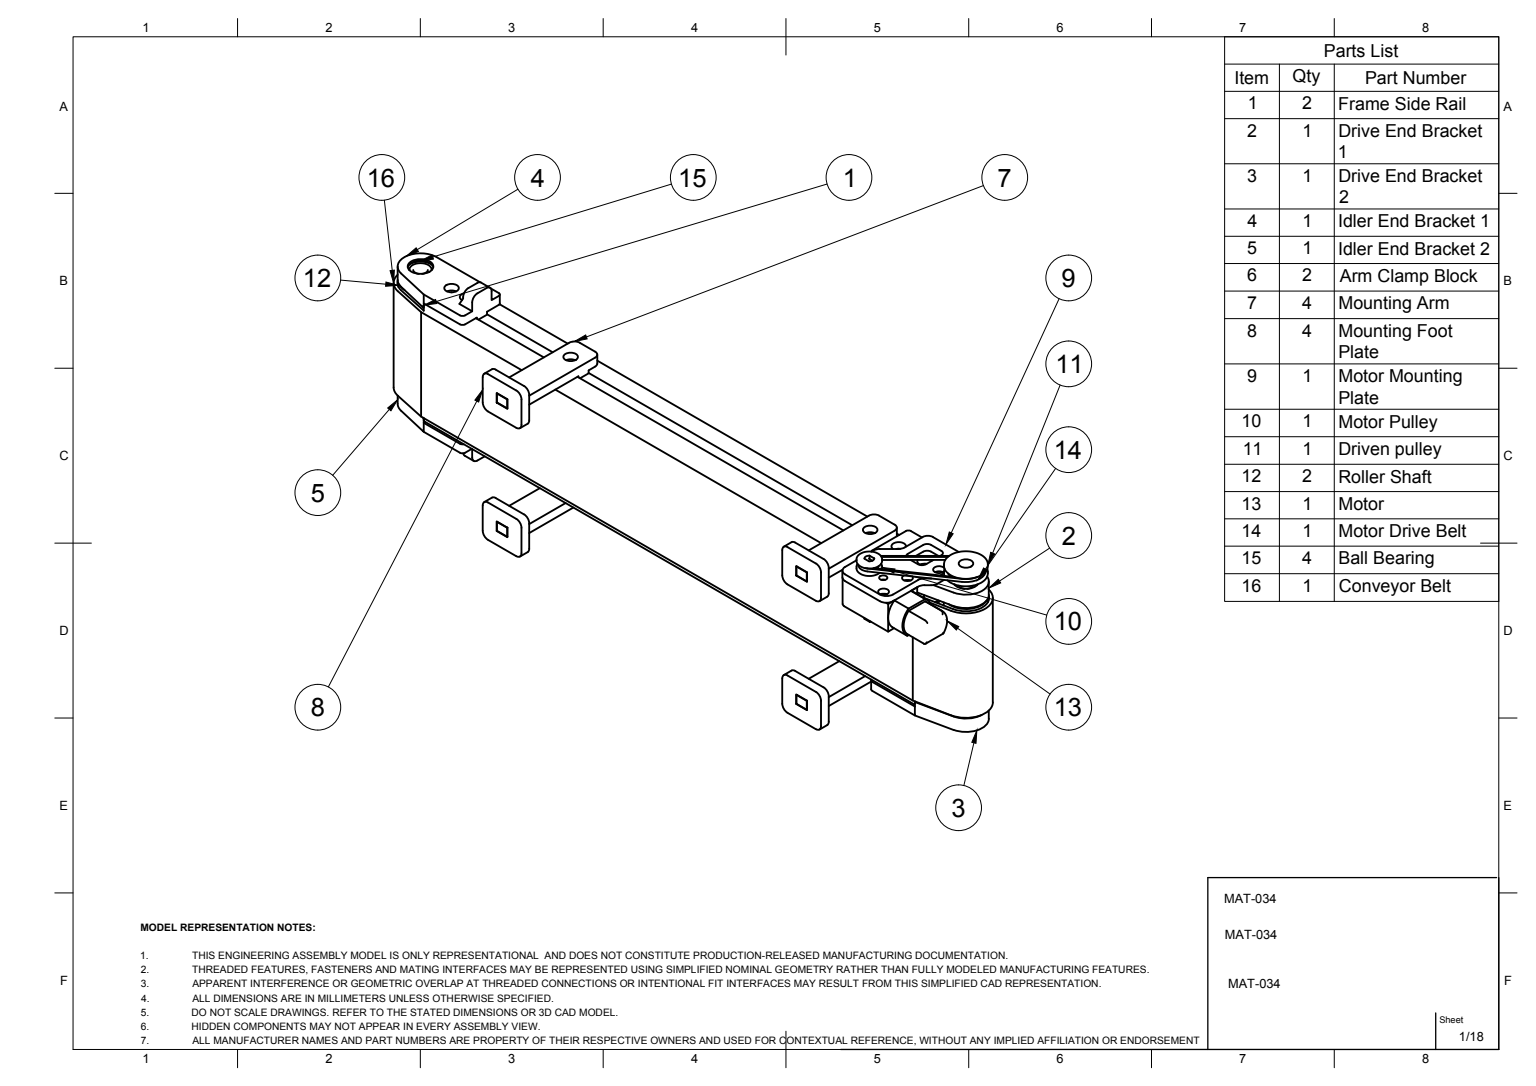
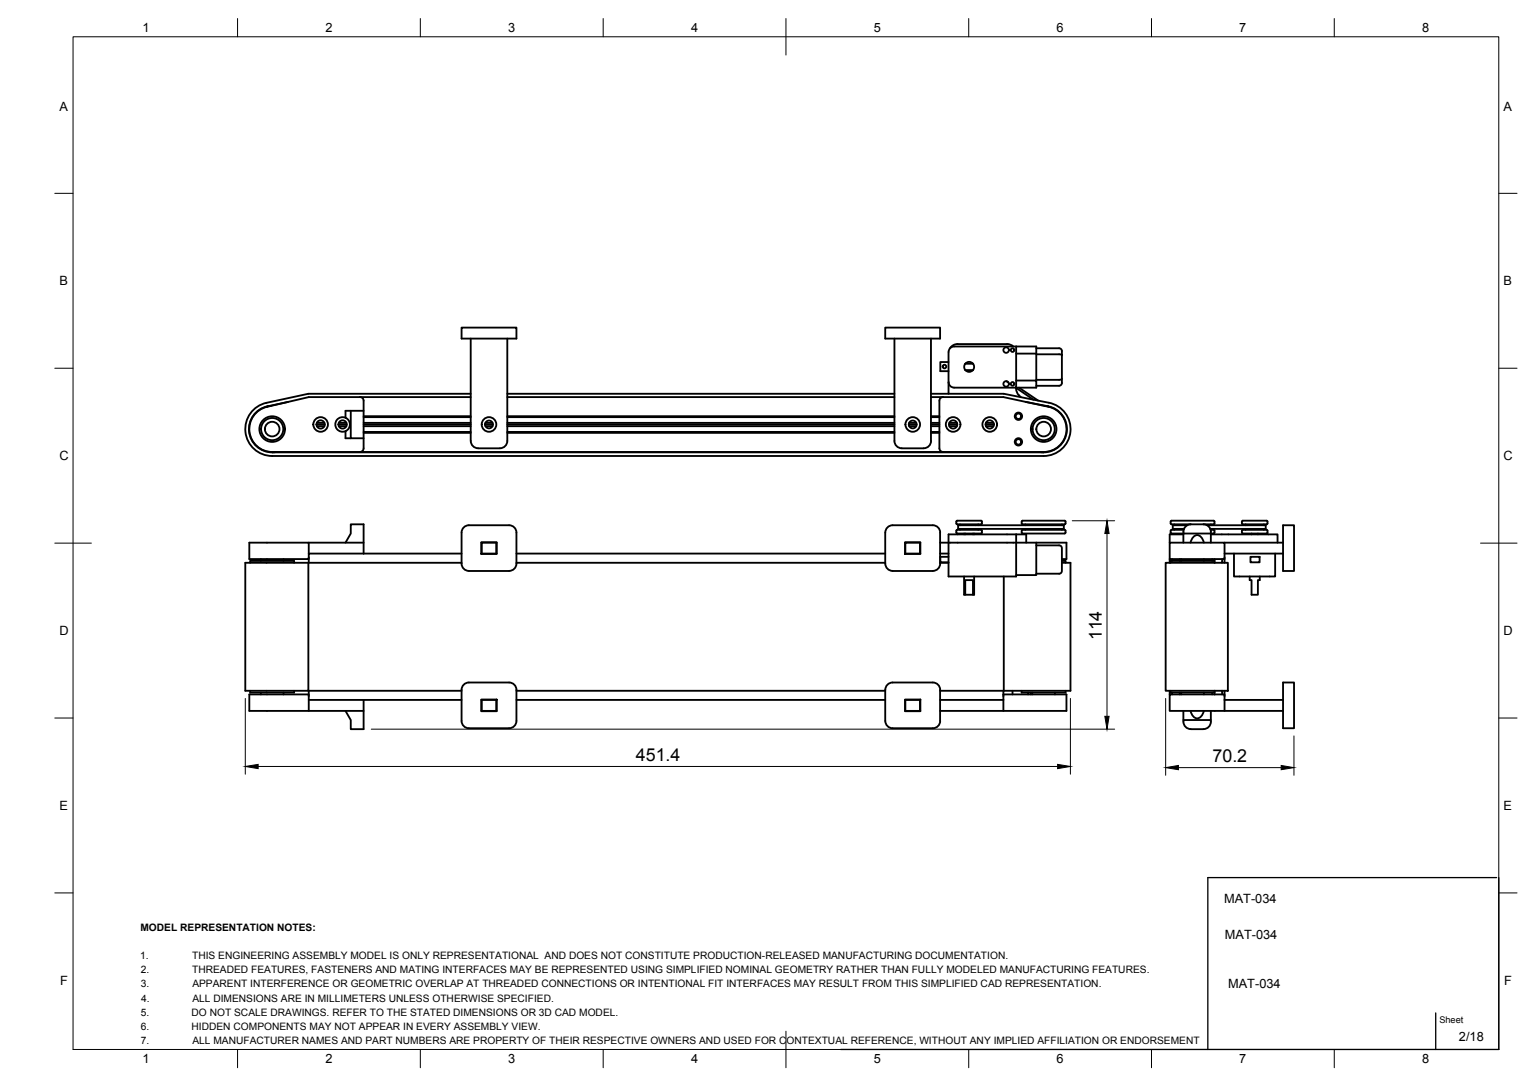
ISO-10303-21;
HEADER;
/* Generated by software containing ST-Developer
 * from STEP Tools, Inc. (www.steptools.com) 
 */

FILE_DESCRIPTION(
/* description */ ('STEP AP214'),
/* implementation_level */ '2;1');

FILE_NAME(
/* name */ 'MAT-034.step',
/* time_stamp */ '2026-11-14T09:24:36-08:00',
/* author */ (''),
/* organization */ (''),
/* preprocessor_version */ 'ST-DEVELOPER v20.2',
/* originating_system */ 'Autodesk Translation Framework v15.17.0.0',
/* authorisation */ '');

FILE_SCHEMA (('AUTOMOTIVE_DESIGN { 1 0 10303 214 3 1 1 }'));
ENDSEC;

DATA;
#10=MECHANICAL_DESIGN_GEOMETRIC_PRESENTATION_REPRESENTATION('',(#203,#204,
#205,#206,#207,#208,#209,#210,#211,#212,#213,#214,#215,#216,#217,#218,#219,
#220,#221,#222,#223,#224,#225,#226),#18867);
#11=ITEM_DEFINED_TRANSFORMATION($,$,#11712,#12275);
#12=ITEM_DEFINED_TRANSFORMATION($,$,#11160,#12276);
#13=ITEM_DEFINED_TRANSFORMATION($,$,#11233,#12277);
#14=ITEM_DEFINED_TRANSFORMATION($,$,#11306,#12278);
#15=ITEM_DEFINED_TRANSFORMATION($,$,#11366,#12279);
#16=ITEM_DEFINED_TRANSFORMATION($,$,#12015,#12280);
#17=ITEM_DEFINED_TRANSFORMATION($,$,#12084,#12281);
#18=ITEM_DEFINED_TRANSFORMATION($,$,#12112,#12282);
#19=ITEM_DEFINED_TRANSFORMATION($,$,#11426,#12283);
#20=ITEM_DEFINED_TRANSFORMATION($,$,#11511,#12284);
#21=ITEM_DEFINED_TRANSFORMATION($,$,#11547,#12285);
#22=ITEM_DEFINED_TRANSFORMATION($,$,#12135,#12286);
#23=ITEM_DEFINED_TRANSFORMATION($,$,#11578,#12287);
#24=ITEM_DEFINED_TRANSFORMATION($,$,#11670,#12288);
#25=ITEM_DEFINED_TRANSFORMATION($,$,#12163,#12289);
#26=ITEM_DEFINED_TRANSFORMATION($,$,#11689,#12290);
#27=ITEM_DEFINED_TRANSFORMATION($,$,#11712,#12291);
#28=ITEM_DEFINED_TRANSFORMATION($,$,#12015,#12292);
#29=ITEM_DEFINED_TRANSFORMATION($,$,#12084,#12293);
#30=ITEM_DEFINED_TRANSFORMATION($,$,#12084,#12294);
#31=ITEM_DEFINED_TRANSFORMATION($,$,#12084,#12295);
#32=ITEM_DEFINED_TRANSFORMATION($,$,#12112,#12296);
#33=ITEM_DEFINED_TRANSFORMATION($,$,#12112,#12297);
#34=ITEM_DEFINED_TRANSFORMATION($,$,#12112,#12298);
#35=ITEM_DEFINED_TRANSFORMATION($,$,#12135,#12299);
#36=ITEM_DEFINED_TRANSFORMATION($,$,#12163,#12300);
#37=ITEM_DEFINED_TRANSFORMATION($,$,#12163,#12301);
#38=ITEM_DEFINED_TRANSFORMATION($,$,#12163,#12302);
#39=(
REPRESENTATION_RELATIONSHIP($,$,#18945,#18934)
REPRESENTATION_RELATIONSHIP_WITH_TRANSFORMATION(#11)
SHAPE_REPRESENTATION_RELATIONSHIP()
);
#40=(
REPRESENTATION_RELATIONSHIP($,$,#18935,#18934)
REPRESENTATION_RELATIONSHIP_WITH_TRANSFORMATION(#12)
SHAPE_REPRESENTATION_RELATIONSHIP()
);
#41=(
REPRESENTATION_RELATIONSHIP($,$,#18936,#18934)
REPRESENTATION_RELATIONSHIP_WITH_TRANSFORMATION(#13)
SHAPE_REPRESENTATION_RELATIONSHIP()
);
#42=(
REPRESENTATION_RELATIONSHIP($,$,#18937,#18934)
REPRESENTATION_RELATIONSHIP_WITH_TRANSFORMATION(#14)
SHAPE_REPRESENTATION_RELATIONSHIP()
);
#43=(
REPRESENTATION_RELATIONSHIP($,$,#18938,#18934)
REPRESENTATION_RELATIONSHIP_WITH_TRANSFORMATION(#15)
SHAPE_REPRESENTATION_RELATIONSHIP()
);
#44=(
REPRESENTATION_RELATIONSHIP($,$,#18946,#18934)
REPRESENTATION_RELATIONSHIP_WITH_TRANSFORMATION(#16)
SHAPE_REPRESENTATION_RELATIONSHIP()
);
#45=(
REPRESENTATION_RELATIONSHIP($,$,#18947,#18934)
REPRESENTATION_RELATIONSHIP_WITH_TRANSFORMATION(#17)
SHAPE_REPRESENTATION_RELATIONSHIP()
);
#46=(
REPRESENTATION_RELATIONSHIP($,$,#18948,#18934)
REPRESENTATION_RELATIONSHIP_WITH_TRANSFORMATION(#18)
SHAPE_REPRESENTATION_RELATIONSHIP()
);
#47=(
REPRESENTATION_RELATIONSHIP($,$,#18939,#18934)
REPRESENTATION_RELATIONSHIP_WITH_TRANSFORMATION(#19)
SHAPE_REPRESENTATION_RELATIONSHIP()
);
#48=(
REPRESENTATION_RELATIONSHIP($,$,#18940,#18934)
REPRESENTATION_RELATIONSHIP_WITH_TRANSFORMATION(#20)
SHAPE_REPRESENTATION_RELATIONSHIP()
);
#49=(
REPRESENTATION_RELATIONSHIP($,$,#18941,#18934)
REPRESENTATION_RELATIONSHIP_WITH_TRANSFORMATION(#21)
SHAPE_REPRESENTATION_RELATIONSHIP()
);
#50=(
REPRESENTATION_RELATIONSHIP($,$,#18949,#18934)
REPRESENTATION_RELATIONSHIP_WITH_TRANSFORMATION(#22)
SHAPE_REPRESENTATION_RELATIONSHIP()
);
#51=(
REPRESENTATION_RELATIONSHIP($,$,#18942,#18934)
REPRESENTATION_RELATIONSHIP_WITH_TRANSFORMATION(#23)
SHAPE_REPRESENTATION_RELATIONSHIP()
);
#52=(
REPRESENTATION_RELATIONSHIP($,$,#18943,#18934)
REPRESENTATION_RELATIONSHIP_WITH_TRANSFORMATION(#24)
SHAPE_REPRESENTATION_RELATIONSHIP()
);
#53=(
REPRESENTATION_RELATIONSHIP($,$,#18950,#18934)
REPRESENTATION_RELATIONSHIP_WITH_TRANSFORMATION(#25)
SHAPE_REPRESENTATION_RELATIONSHIP()
);
#54=(
REPRESENTATION_RELATIONSHIP($,$,#18944,#18934)
REPRESENTATION_RELATIONSHIP_WITH_TRANSFORMATION(#26)
SHAPE_REPRESENTATION_RELATIONSHIP()
);
#55=(
REPRESENTATION_RELATIONSHIP($,$,#18945,#18934)
REPRESENTATION_RELATIONSHIP_WITH_TRANSFORMATION(#27)
SHAPE_REPRESENTATION_RELATIONSHIP()
);
#56=(
REPRESENTATION_RELATIONSHIP($,$,#18946,#18934)
REPRESENTATION_RELATIONSHIP_WITH_TRANSFORMATION(#28)
SHAPE_REPRESENTATION_RELATIONSHIP()
);
#57=(
REPRESENTATION_RELATIONSHIP($,$,#18947,#18934)
REPRESENTATION_RELATIONSHIP_WITH_TRANSFORMATION(#29)
SHAPE_REPRESENTATION_RELATIONSHIP()
);
#58=(
REPRESENTATION_RELATIONSHIP($,$,#18947,#18934)
REPRESENTATION_RELATIONSHIP_WITH_TRANSFORMATION(#30)
SHAPE_REPRESENTATION_RELATIONSHIP()
);
#59=(
REPRESENTATION_RELATIONSHIP($,$,#18947,#18934)
REPRESENTATION_RELATIONSHIP_WITH_TRANSFORMATION(#31)
SHAPE_REPRESENTATION_RELATIONSHIP()
);
#60=(
REPRESENTATION_RELATIONSHIP($,$,#18948,#18934)
REPRESENTATION_RELATIONSHIP_WITH_TRANSFORMATION(#32)
SHAPE_REPRESENTATION_RELATIONSHIP()
);
#61=(
REPRESENTATION_RELATIONSHIP($,$,#18948,#18934)
REPRESENTATION_RELATIONSHIP_WITH_TRANSFORMATION(#33)
SHAPE_REPRESENTATION_RELATIONSHIP()
);
#62=(
REPRESENTATION_RELATIONSHIP($,$,#18948,#18934)
REPRESENTATION_RELATIONSHIP_WITH_TRANSFORMATION(#34)
SHAPE_REPRESENTATION_RELATIONSHIP()
);
#63=(
REPRESENTATION_RELATIONSHIP($,$,#18949,#18934)
REPRESENTATION_RELATIONSHIP_WITH_TRANSFORMATION(#35)
SHAPE_REPRESENTATION_RELATIONSHIP()
);
#64=(
REPRESENTATION_RELATIONSHIP($,$,#18950,#18934)
REPRESENTATION_RELATIONSHIP_WITH_TRANSFORMATION(#36)
SHAPE_REPRESENTATION_RELATIONSHIP()
);
#65=(
REPRESENTATION_RELATIONSHIP($,$,#18950,#18934)
REPRESENTATION_RELATIONSHIP_WITH_TRANSFORMATION(#37)
SHAPE_REPRESENTATION_RELATIONSHIP()
);
#66=(
REPRESENTATION_RELATIONSHIP($,$,#18950,#18934)
REPRESENTATION_RELATIONSHIP_WITH_TRANSFORMATION(#38)
SHAPE_REPRESENTATION_RELATIONSHIP()
);
#67=CONTEXT_DEPENDENT_SHAPE_REPRESENTATION(#39,#18906);
#68=CONTEXT_DEPENDENT_SHAPE_REPRESENTATION(#40,#18907);
#69=CONTEXT_DEPENDENT_SHAPE_REPRESENTATION(#41,#18908);
#70=CONTEXT_DEPENDENT_SHAPE_REPRESENTATION(#42,#18909);
#71=CONTEXT_DEPENDENT_SHAPE_REPRESENTATION(#43,#18910);
#72=CONTEXT_DEPENDENT_SHAPE_REPRESENTATION(#44,#18911);
#73=CONTEXT_DEPENDENT_SHAPE_REPRESENTATION(#45,#18912);
#74=CONTEXT_DEPENDENT_SHAPE_REPRESENTATION(#46,#18913);
#75=CONTEXT_DEPENDENT_SHAPE_REPRESENTATION(#47,#18914);
#76=CONTEXT_DEPENDENT_SHAPE_REPRESENTATION(#48,#18915);
#77=CONTEXT_DEPENDENT_SHAPE_REPRESENTATION(#49,#18916);
#78=CONTEXT_DEPENDENT_SHAPE_REPRESENTATION(#50,#18917);
#79=CONTEXT_DEPENDENT_SHAPE_REPRESENTATION(#51,#18918);
#80=CONTEXT_DEPENDENT_SHAPE_REPRESENTATION(#52,#18919);
#81=CONTEXT_DEPENDENT_SHAPE_REPRESENTATION(#53,#18920);
#82=CONTEXT_DEPENDENT_SHAPE_REPRESENTATION(#54,#18921);
#83=CONTEXT_DEPENDENT_SHAPE_REPRESENTATION(#55,#18922);
#84=CONTEXT_DEPENDENT_SHAPE_REPRESENTATION(#56,#18923);
#85=CONTEXT_DEPENDENT_SHAPE_REPRESENTATION(#57,#18924);
#86=CONTEXT_DEPENDENT_SHAPE_REPRESENTATION(#58,#18925);
#87=CONTEXT_DEPENDENT_SHAPE_REPRESENTATION(#59,#18926);
#88=CONTEXT_DEPENDENT_SHAPE_REPRESENTATION(#60,#18927);
#89=CONTEXT_DEPENDENT_SHAPE_REPRESENTATION(#61,#18928);
#90=CONTEXT_DEPENDENT_SHAPE_REPRESENTATION(#62,#18929);
#91=CONTEXT_DEPENDENT_SHAPE_REPRESENTATION(#63,#18930);
#92=CONTEXT_DEPENDENT_SHAPE_REPRESENTATION(#64,#18931);
#93=CONTEXT_DEPENDENT_SHAPE_REPRESENTATION(#65,#18932);
#94=CONTEXT_DEPENDENT_SHAPE_REPRESENTATION(#66,#18933);
#95=NEXT_ASSEMBLY_USAGE_OCCURRENCE('Frame Side Rail:1',
'Frame Side Rail:1','Frame Side Rail:1',#18952,#18963,
'Frame Side Rail:1');
#96=NEXT_ASSEMBLY_USAGE_OCCURRENCE('Drive End Bracket 1:1',
'Drive End Bracket 1:1','Drive End Bracket 1:1',#18952,#18953,
'Drive End Bracket 1:1');
#97=NEXT_ASSEMBLY_USAGE_OCCURRENCE('Drive End Bracket 2:1',
'Drive End Bracket 2:1','Drive End Bracket 2:1',#18952,#18954,
'Drive End Bracket 2:1');
#98=NEXT_ASSEMBLY_USAGE_OCCURRENCE('Idler End Bracket 1:1',
'Idler End Bracket 1:1','Idler End Bracket 1:1',#18952,#18955,
'Idler End Bracket 1:1');
#99=NEXT_ASSEMBLY_USAGE_OCCURRENCE('Idler End Bracket 2:1',
'Idler End Bracket 2:1','Idler End Bracket 2:1',#18952,#18956,
'Idler End Bracket 2:1');
#100=NEXT_ASSEMBLY_USAGE_OCCURRENCE('Arm Clamp Block:1',
'Arm Clamp Block:1','Arm Clamp Block:1',#18952,#18964,
'Arm Clamp Block:1');
#101=NEXT_ASSEMBLY_USAGE_OCCURRENCE('Mounting Arm:1','Mounting Arm:1',
'Mounting Arm:1',#18952,#18965,'Mounting Arm:1');
#102=NEXT_ASSEMBLY_USAGE_OCCURRENCE('Mounting Foot Plate:1',
'Mounting Foot Plate:1','Mounting Foot Plate:1',#18952,#18966,
'Mounting Foot Plate:1');
#103=NEXT_ASSEMBLY_USAGE_OCCURRENCE('Motor Mounting Plate:1',
'Motor Mounting Plate:1','Motor Mounting Plate:1',#18952,#18957,
'Motor Mounting Plate:1');
#104=NEXT_ASSEMBLY_USAGE_OCCURRENCE('Motor Pulley:1','Motor Pulley:1',
'Motor Pulley:1',#18952,#18958,'Motor Pulley:1');
#105=NEXT_ASSEMBLY_USAGE_OCCURRENCE('Driven Pulley:1','Driven Pulley:1',
'Driven Pulley:1',#18952,#18959,'Driven Pulley:1');
#106=NEXT_ASSEMBLY_USAGE_OCCURRENCE('Roller Shaft:1','Roller Shaft:1',
'Roller Shaft:1',#18952,#18967,'Roller Shaft:1');
#107=NEXT_ASSEMBLY_USAGE_OCCURRENCE('Motor:1','Motor:1','Motor:1',#18952,
#18960,'Motor:1');
#108=NEXT_ASSEMBLY_USAGE_OCCURRENCE('Motor Drive Belt:1',
'Motor Drive Belt:1','Motor Drive Belt:1',#18952,#18961,
'Motor Drive Belt:1');
#109=NEXT_ASSEMBLY_USAGE_OCCURRENCE('Ball Bearing:1','Ball Bearing:1',
'Ball Bearing:1',#18952,#18968,'Ball Bearing:1');
#110=NEXT_ASSEMBLY_USAGE_OCCURRENCE('Conveyor Belt:1','Conveyor Belt:1',
'Conveyor Belt:1',#18952,#18962,'Conveyor Belt:1');
#111=NEXT_ASSEMBLY_USAGE_OCCURRENCE('Frame Side Rail:2',
'Frame Side Rail:2','Frame Side Rail:2',#18952,#18963,
'Frame Side Rail:2');
#112=NEXT_ASSEMBLY_USAGE_OCCURRENCE('Arm Clamp Block:2',
'Arm Clamp Block:2','Arm Clamp Block:2',#18952,#18964,
'Arm Clamp Block:2');
#113=NEXT_ASSEMBLY_USAGE_OCCURRENCE('Mounting Arm:2','Mounting Arm:2',
'Mounting Arm:2',#18952,#18965,'Mounting Arm:2');
#114=NEXT_ASSEMBLY_USAGE_OCCURRENCE('Mounting Arm:3','Mounting Arm:3',
'Mounting Arm:3',#18952,#18965,'Mounting Arm:3');
#115=NEXT_ASSEMBLY_USAGE_OCCURRENCE('Mounting Arm:4','Mounting Arm:4',
'Mounting Arm:4',#18952,#18965,'Mounting Arm:4');
#116=NEXT_ASSEMBLY_USAGE_OCCURRENCE('Mounting Foot Plate:2',
'Mounting Foot Plate:2','Mounting Foot Plate:2',#18952,#18966,
'Mounting Foot Plate:2');
#117=NEXT_ASSEMBLY_USAGE_OCCURRENCE('Mounting Foot Plate:3',
'Mounting Foot Plate:3','Mounting Foot Plate:3',#18952,#18966,
'Mounting Foot Plate:3');
#118=NEXT_ASSEMBLY_USAGE_OCCURRENCE('Mounting Foot Plate:4',
'Mounting Foot Plate:4','Mounting Foot Plate:4',#18952,#18966,
'Mounting Foot Plate:4');
#119=NEXT_ASSEMBLY_USAGE_OCCURRENCE('Roller Shaft:2','Roller Shaft:2',
'Roller Shaft:2',#18952,#18967,'Roller Shaft:2');
#120=NEXT_ASSEMBLY_USAGE_OCCURRENCE('Ball Bearing:2','Ball Bearing:2',
'Ball Bearing:2',#18952,#18968,'Ball Bearing:2');
#121=NEXT_ASSEMBLY_USAGE_OCCURRENCE('Ball Bearing:3','Ball Bearing:3',
'Ball Bearing:3',#18952,#18968,'Ball Bearing:3');
#122=NEXT_ASSEMBLY_USAGE_OCCURRENCE('Ball Bearing:4','Ball Bearing:4',
'Ball Bearing:4',#18952,#18968,'Ball Bearing:4');
#123=SPHERICAL_SURFACE('',#12164,1.9845);
#124=SPHERICAL_SURFACE('',#12166,1.9845);
#125=SPHERICAL_SURFACE('',#12168,1.9845);
#126=SPHERICAL_SURFACE('',#12170,1.9845);
#127=SPHERICAL_SURFACE('',#12172,1.9845);
#128=SPHERICAL_SURFACE('',#12174,1.9845);
#129=SPHERICAL_SURFACE('',#12176,1.9845);
#130=CONICAL_SURFACE('',#12139,12.7,0.0194419944400805);
#131=CONICAL_SURFACE('',#12143,12.7,0.0194419944400803);
#132=CONICAL_SURFACE('',#12193,8.8,1.39626340159546);
#133=CONICAL_SURFACE('',#12203,9.6,1.39626340159547);
#134=CONICAL_SURFACE('',#12217,9.6,1.46902152746005);
#135=CONICAL_SURFACE('',#12222,8.71875,1.51977681092793);
#136=CONICAL_SURFACE('',#12225,7.8375,1.51977681092793);
#137=CONICAL_SURFACE('',#12227,7.8375,1.51977681092793);
#138=CONICAL_SURFACE('',#12231,8.71875,1.46902152746005);
#139=CONICAL_SURFACE('',#12235,6.075,1.51977681092793);
#140=CONICAL_SURFACE('',#12238,8.71875,1.51977681092792);
#141=CONICAL_SURFACE('',#12242,9.6,1.51977681092792);
#142=B_SPLINE_CURVE_WITH_KNOTS('',3,(#16841,#16842,#16843,#16844,#16845,
#16846,#16847,#16848,#16849,#16850,#16851,#16852,#16853,#16854),
 .UNSPECIFIED.,.F.,.F.,(4,2,2,2,2,2,4),(0.245799129465821,0.300704982929502,
0.357513955396153,0.418543136612542,0.45489286030411,0.491598258931638,
0.492200531214483),.UNSPECIFIED.);
#143=B_SPLINE_CURVE_WITH_KNOTS('',3,(#16857,#16858,#16859,#16860,#16861,
#16862,#16863,#16864,#16865,#16866,#16867,#16868,#16869,#16870),
 .UNSPECIFIED.,.F.,.F.,(4,2,2,2,2,2,4),(-0.243764588636152,-0.188160877929009,
-0.130985417478992,-0.0703706382818566,-0.0353193180725583,0.,0.000595335954832901),
 .UNSPECIFIED.);
#144=B_SPLINE_CURVE_WITH_KNOTS('',3,(#17002,#17003,#17004,#17005,#17006,
#17007,#17008,#17009,#17010,#17011,#17012,#17013,#17014,#17015),
 .UNSPECIFIED.,.F.,.F.,(4,2,2,2,2,2,4),(-0.000602272282836634,0.,0.0367053986270638,
0.0730551223181225,0.134084303533662,0.190893275999521,0.245799129462431),
 .UNSPECIFIED.);
#145=B_SPLINE_CURVE_WITH_KNOTS('',3,(#17017,#17018,#17019,#17020,#17021,
#17022,#17023,#17024,#17025,#17026,#17027,#17028,#17029,#17030),
 .UNSPECIFIED.,.F.,.F.,(4,2,2,2,2,2,4),(-0.488124513225642,-0.487529177270534,
-0.452209859198347,-0.417158538989302,-0.356543759792373,-0.299368299342555,
-0.243764588635598),.UNSPECIFIED.);
#146=TOROIDAL_SURFACE('',#11512,6.5,0.5);
#147=TOROIDAL_SURFACE('',#11516,6.5,0.5);
#148=TOROIDAL_SURFACE('',#11521,6.5,0.5);
#149=TOROIDAL_SURFACE('',#11525,6.5,0.5);
#150=TOROIDAL_SURFACE('',#11551,11.5,0.5);
#151=TOROIDAL_SURFACE('',#11555,11.5,0.5);
#152=TOROIDAL_SURFACE('',#11560,11.5,0.5);
#153=TOROIDAL_SURFACE('',#11564,11.5,0.5);
#154=TOROIDAL_SURFACE('',#11579,1.8,0.2);
#155=TOROIDAL_SURFACE('',#11608,8.75000000000038,1.5);
#156=TOROIDAL_SURFACE('',#11653,8.75000000000038,1.5);
#157=TOROIDAL_SURFACE('',#12178,10.7,0.3);
#158=TOROIDAL_SURFACE('',#12184,10.7,0.3);
#159=TOROIDAL_SURFACE('',#12190,9.6,0.18);
#160=TOROIDAL_SURFACE('',#12197,7.35,1.9845);
#161=TOROIDAL_SURFACE('',#12206,9.6,0.18);
#162=TOROIDAL_SURFACE('',#12213,7.35,1.9845);
#163=TOROIDAL_SURFACE('',#12250,5.975,0.1);
#164=TOROIDAL_SURFACE('',#12253,4.3,0.3);
#165=TOROIDAL_SURFACE('',#12259,4.3,0.3);
#166=TOROIDAL_SURFACE('',#12262,5.975,0.1);
#167=ELLIPSE('',#11309,7.99999999999913,3.99999999999963);
#168=ELLIPSE('',#11311,7.99999999999913,3.99999999999963);
#169=ELLIPSE('',#11369,7.99999999999924,3.99999999999989);
#170=ELLIPSE('',#11371,7.99999999999924,3.99999999999989);
#171=SHAPE_REPRESENTATION_RELATIONSHIP('SRR','None',#18935,#187);
#172=SHAPE_REPRESENTATION_RELATIONSHIP('SRR','None',#18936,#188);
#173=SHAPE_REPRESENTATION_RELATIONSHIP('SRR','None',#18937,#189);
#174=SHAPE_REPRESENTATION_RELATIONSHIP('SRR','None',#18938,#190);
#175=SHAPE_REPRESENTATION_RELATIONSHIP('SRR','None',#18939,#191);
#176=SHAPE_REPRESENTATION_RELATIONSHIP('SRR','None',#18940,#192);
#177=SHAPE_REPRESENTATION_RELATIONSHIP('SRR','None',#18941,#193);
#178=SHAPE_REPRESENTATION_RELATIONSHIP('SRR','None',#18942,#194);
#179=SHAPE_REPRESENTATION_RELATIONSHIP('SRR','None',#18943,#195);
#180=SHAPE_REPRESENTATION_RELATIONSHIP('SRR','None',#18944,#196);
#181=SHAPE_REPRESENTATION_RELATIONSHIP('SRR','None',#18945,#197);
#182=SHAPE_REPRESENTATION_RELATIONSHIP('SRR','None',#18946,#198);
#183=SHAPE_REPRESENTATION_RELATIONSHIP('SRR','None',#18947,#199);
#184=SHAPE_REPRESENTATION_RELATIONSHIP('SRR','None',#18948,#200);
#185=SHAPE_REPRESENTATION_RELATIONSHIP('SRR','None',#18949,#201);
#186=SHAPE_REPRESENTATION_RELATIONSHIP('SRR','None',#18950,#202);
#187=ADVANCED_BREP_SHAPE_REPRESENTATION('',(#227),#18851);
#188=ADVANCED_BREP_SHAPE_REPRESENTATION('',(#228),#18852);
#189=ADVANCED_BREP_SHAPE_REPRESENTATION('',(#229),#18853);
#190=ADVANCED_BREP_SHAPE_REPRESENTATION('',(#230),#18854);
#191=ADVANCED_BREP_SHAPE_REPRESENTATION('',(#231),#18855);
#192=ADVANCED_BREP_SHAPE_REPRESENTATION('',(#232),#18856);
#193=ADVANCED_BREP_SHAPE_REPRESENTATION('',(#233),#18857);
#194=ADVANCED_BREP_SHAPE_REPRESENTATION('',(#234),#18858);
#195=ADVANCED_BREP_SHAPE_REPRESENTATION('',(#235),#18859);
#196=ADVANCED_BREP_SHAPE_REPRESENTATION('',(#236),#18860);
#197=ADVANCED_BREP_SHAPE_REPRESENTATION('',(#237),#18861);
#198=ADVANCED_BREP_SHAPE_REPRESENTATION('',(#238),#18862);
#199=ADVANCED_BREP_SHAPE_REPRESENTATION('',(#239),#18863);
#200=ADVANCED_BREP_SHAPE_REPRESENTATION('',(#240),#18864);
#201=ADVANCED_BREP_SHAPE_REPRESENTATION('',(#241),#18865);
#202=ADVANCED_BREP_SHAPE_REPRESENTATION('',(#242,#243,#244,#245,#246,#247,
#248,#249,#250),#18866);
#203=STYLED_ITEM('',(#19024),#227);
#204=STYLED_ITEM('',(#19024),#228);
#205=STYLED_ITEM('',(#19024),#229);
#206=STYLED_ITEM('',(#19025),#230);
#207=STYLED_ITEM('',(#19026),#231);
#208=STYLED_ITEM('',(#19027),#232);
#209=STYLED_ITEM('',(#19027),#233);
#210=STYLED_ITEM('',(#19026),#234);
#211=STYLED_ITEM('',(#19028),#235);
#212=STYLED_ITEM('',(#19028),#236);
#213=STYLED_ITEM('',(#19024),#237);
#214=STYLED_ITEM('',(#19026),#238);
#215=STYLED_ITEM('',(#19026),#239);
#216=STYLED_ITEM('',(#19024),#240);
#217=STYLED_ITEM('',(#19027),#241);
#218=STYLED_ITEM('',(#19027),#242);
#219=STYLED_ITEM('',(#19027),#243);
#220=STYLED_ITEM('',(#19027),#244);
#221=STYLED_ITEM('',(#19027),#245);
#222=STYLED_ITEM('',(#19027),#246);
#223=STYLED_ITEM('',(#19027),#247);
#224=STYLED_ITEM('',(#19027),#248);
#225=STYLED_ITEM('',(#19027),#249);
#226=STYLED_ITEM('',(#19027),#250);
#227=MANIFOLD_SOLID_BREP('Body1',#10958);
#228=MANIFOLD_SOLID_BREP('Body1',#10959);
#229=MANIFOLD_SOLID_BREP('Body1',#10960);
#230=MANIFOLD_SOLID_BREP('Body1',#10961);
#231=MANIFOLD_SOLID_BREP('Body1',#10962);
#232=MANIFOLD_SOLID_BREP('Body1',#10963);
#233=MANIFOLD_SOLID_BREP('Body1',#10964);
#234=MANIFOLD_SOLID_BREP('Body1',#10965);
#235=MANIFOLD_SOLID_BREP('Body1',#10966);
#236=MANIFOLD_SOLID_BREP('Body1',#10967);
#237=MANIFOLD_SOLID_BREP('Body1',#10968);
#238=MANIFOLD_SOLID_BREP('Body1',#10969);
#239=MANIFOLD_SOLID_BREP('Body1',#10970);
#240=MANIFOLD_SOLID_BREP('Body1',#10971);
#241=MANIFOLD_SOLID_BREP('Body1',#10972);
#242=MANIFOLD_SOLID_BREP('Body1',#10973);
#243=MANIFOLD_SOLID_BREP('Body2',#10974);
#244=MANIFOLD_SOLID_BREP('Body3',#10975);
#245=MANIFOLD_SOLID_BREP('Body4',#10976);
#246=MANIFOLD_SOLID_BREP('Body5',#10977);
#247=MANIFOLD_SOLID_BREP('Body6',#10978);
#248=MANIFOLD_SOLID_BREP('Body7',#10979);
#249=MANIFOLD_SOLID_BREP('Body8',#10980);
#250=MANIFOLD_SOLID_BREP('Body9',#10981);
#251=FACE_BOUND('',#1334,.T.);
#252=FACE_BOUND('',#1335,.T.);
#253=FACE_BOUND('',#1336,.T.);
#254=FACE_BOUND('',#1343,.T.);
#255=FACE_BOUND('',#1344,.T.);
#256=FACE_BOUND('',#1345,.T.);
#257=FACE_BOUND('',#1346,.T.);
#258=FACE_BOUND('',#1347,.T.);
#259=FACE_BOUND('',#1349,.T.);
#260=FACE_BOUND('',#1351,.T.);
#261=FACE_BOUND('',#1358,.T.);
#262=FACE_BOUND('',#1360,.T.);
#263=FACE_BOUND('',#1368,.T.);
#264=FACE_BOUND('',#1376,.T.);
#265=FACE_BOUND('',#1381,.T.);
#266=FACE_BOUND('',#1382,.T.);
#267=FACE_BOUND('',#1398,.T.);
#268=FACE_BOUND('',#1399,.T.);
#269=FACE_BOUND('',#1400,.T.);
#270=FACE_BOUND('',#1407,.T.);
#271=FACE_BOUND('',#1408,.T.);
#272=FACE_BOUND('',#1409,.T.);
#273=FACE_BOUND('',#1410,.T.);
#274=FACE_BOUND('',#1411,.T.);
#275=FACE_BOUND('',#1413,.T.);
#276=FACE_BOUND('',#1415,.T.);
#277=FACE_BOUND('',#1422,.T.);
#278=FACE_BOUND('',#1424,.T.);
#279=FACE_BOUND('',#1432,.T.);
#280=FACE_BOUND('',#1440,.T.);
#281=FACE_BOUND('',#1445,.T.);
#282=FACE_BOUND('',#1446,.T.);
#283=FACE_BOUND('',#1465,.T.);
#284=FACE_BOUND('',#1466,.T.);
#285=FACE_BOUND('',#1468,.T.);
#286=FACE_BOUND('',#1470,.T.);
#287=FACE_BOUND('',#1472,.T.);
#288=FACE_BOUND('',#1476,.T.);
#289=FACE_BOUND('',#1478,.T.);
#290=FACE_BOUND('',#1487,.T.);
#291=FACE_BOUND('',#1488,.T.);
#292=FACE_BOUND('',#1507,.T.);
#293=FACE_BOUND('',#1508,.T.);
#294=FACE_BOUND('',#1510,.T.);
#295=FACE_BOUND('',#1512,.T.);
#296=FACE_BOUND('',#1514,.T.);
#297=FACE_BOUND('',#1518,.T.);
#298=FACE_BOUND('',#1520,.T.);
#299=FACE_BOUND('',#1529,.T.);
#300=FACE_BOUND('',#1530,.T.);
#301=FACE_BOUND('',#1568,.T.);
#302=FACE_BOUND('',#1569,.T.);
#303=FACE_BOUND('',#1570,.T.);
#304=FACE_BOUND('',#1571,.T.);
#305=FACE_BOUND('',#1572,.T.);
#306=FACE_BOUND('',#1573,.T.);
#307=FACE_BOUND('',#1574,.T.);
#308=FACE_BOUND('',#1576,.T.);
#309=FACE_BOUND('',#1578,.T.);
#310=FACE_BOUND('',#1580,.T.);
#311=FACE_BOUND('',#1581,.T.);
#312=FACE_BOUND('',#1582,.T.);
#313=FACE_BOUND('',#1583,.T.);
#314=FACE_BOUND('',#1584,.T.);
#315=FACE_BOUND('',#1585,.T.);
#316=FACE_BOUND('',#1586,.T.);
#317=FACE_BOUND('',#1588,.T.);
#318=FACE_BOUND('',#1590,.T.);
#319=FACE_BOUND('',#1599,.T.);
#320=FACE_BOUND('',#1601,.T.);
#321=FACE_BOUND('',#1603,.T.);
#322=FACE_BOUND('',#1605,.T.);
#323=FACE_BOUND('',#1619,.T.);
#324=FACE_BOUND('',#1621,.T.);
#325=FACE_BOUND('',#1623,.T.);
#326=FACE_BOUND('',#1625,.T.);
#327=FACE_BOUND('',#1639,.T.);
#328=FACE_BOUND('',#1640,.T.);
#329=FACE_BOUND('',#1641,.T.);
#330=FACE_BOUND('',#1642,.T.);
#331=FACE_BOUND('',#1643,.T.);
#332=FACE_BOUND('',#1644,.T.);
#333=FACE_BOUND('',#1646,.T.);
#334=FACE_BOUND('',#1649,.T.);
#335=FACE_BOUND('',#1659,.T.);
#336=FACE_BOUND('',#1660,.T.);
#337=FACE_BOUND('',#1661,.T.);
#338=FACE_BOUND('',#1662,.T.);
#339=FACE_BOUND('',#1663,.T.);
#340=FACE_BOUND('',#1682,.T.);
#341=FACE_BOUND('',#1685,.T.);
#342=FACE_BOUND('',#1692,.T.);
#343=FACE_BOUND('',#1694,.T.);
#344=FACE_BOUND('',#1704,.T.);
#345=FACE_BOUND('',#1706,.T.);
#346=FACE_BOUND('',#1719,.T.);
#347=FACE_BOUND('',#1720,.T.);
#348=FACE_BOUND('',#1721,.T.);
#349=FACE_BOUND('',#1722,.T.);
#350=FACE_BOUND('',#1723,.T.);
#351=FACE_BOUND('',#1725,.T.);
#352=FACE_BOUND('',#1726,.T.);
#353=FACE_BOUND('',#1727,.T.);
#354=FACE_BOUND('',#1728,.T.);
#355=FACE_BOUND('',#1729,.T.);
#356=FACE_BOUND('',#1900,.T.);
#357=FACE_BOUND('',#1905,.T.);
#358=FACE_BOUND('',#1908,.T.);
#359=FACE_BOUND('',#1910,.T.);
#360=FACE_BOUND('',#1924,.T.);
#361=FACE_BOUND('',#1928,.T.);
#362=FACE_BOUND('',#1945,.T.);
#363=FACE_BOUND('',#1952,.T.);
#364=FACE_BOUND('',#1956,.T.);
#365=FACE_BOUND('',#1958,.T.);
#366=FACE_BOUND('',#1960,.T.);
#367=FACE_BOUND('',#1981,.T.);
#368=FACE_BOUND('',#1983,.T.);
#369=FACE_BOUND('',#1985,.T.);
#370=FACE_BOUND('',#1987,.T.);
#371=FACE_BOUND('',#1989,.T.);
#372=FACE_BOUND('',#1991,.T.);
#373=FACE_BOUND('',#2012,.T.);
#374=FACE_BOUND('',#2014,.T.);
#375=FACE_BOUND('',#2036,.T.);
#376=FACE_BOUND('',#2038,.T.);
#377=FACE_BOUND('',#2040,.T.);
#378=FACE_BOUND('',#2042,.T.);
#379=FACE_BOUND('',#2044,.T.);
#380=FACE_BOUND('',#2046,.T.);
#381=PLANE('',#11188);
#382=PLANE('',#11189);
#383=PLANE('',#11191);
#384=PLANE('',#11193);
#385=PLANE('',#11195);
#386=PLANE('',#11198);
#387=PLANE('',#11199);
#388=PLANE('',#11200);
#389=PLANE('',#11201);
#390=PLANE('',#11204);
#391=PLANE('',#11205);
#392=PLANE('',#11206);
#393=PLANE('',#11207);
#394=PLANE('',#11208);
#395=PLANE('',#11211);
#396=PLANE('',#11212);
#397=PLANE('',#11213);
#398=PLANE('',#11214);
#399=PLANE('',#11215);
#400=PLANE('',#11216);
#401=PLANE('',#11217);
#402=PLANE('',#11218);
#403=PLANE('',#11219);
#404=PLANE('',#11220);
#405=PLANE('',#11221);
#406=PLANE('',#11222);
#407=PLANE('',#11223);
#408=PLANE('',#11224);
#409=PLANE('',#11225);
#410=PLANE('',#11226);
#411=PLANE('',#11227);
#412=PLANE('',#11228);
#413=PLANE('',#11229);
#414=PLANE('',#11230);
#415=PLANE('',#11231);
#416=PLANE('',#11232);
#417=PLANE('',#11261);
#418=PLANE('',#11262);
#419=PLANE('',#11264);
#420=PLANE('',#11266);
#421=PLANE('',#11268);
#422=PLANE('',#11271);
#423=PLANE('',#11272);
#424=PLANE('',#11273);
#425=PLANE('',#11274);
#426=PLANE('',#11277);
#427=PLANE('',#11278);
#428=PLANE('',#11279);
#429=PLANE('',#11280);
#430=PLANE('',#11281);
#431=PLANE('',#11284);
#432=PLANE('',#11285);
#433=PLANE('',#11286);
#434=PLANE('',#11287);
#435=PLANE('',#11288);
#436=PLANE('',#11289);
#437=PLANE('',#11290);
#438=PLANE('',#11291);
#439=PLANE('',#11292);
#440=PLANE('',#11293);
#441=PLANE('',#11294);
#442=PLANE('',#11295);
#443=PLANE('',#11296);
#444=PLANE('',#11297);
#445=PLANE('',#11298);
#446=PLANE('',#11299);
#447=PLANE('',#11300);
#448=PLANE('',#11301);
#449=PLANE('',#11302);
#450=PLANE('',#11303);
#451=PLANE('',#11304);
#452=PLANE('',#11305);
#453=PLANE('',#11330);
#454=PLANE('',#11332);
#455=PLANE('',#11334);
#456=PLANE('',#11335);
#457=PLANE('',#11339);
#458=PLANE('',#11340);
#459=PLANE('',#11343);
#460=PLANE('',#11344);
#461=PLANE('',#11347);
#462=PLANE('',#11348);
#463=PLANE('',#11349);
#464=PLANE('',#11352);
#465=PLANE('',#11353);
#466=PLANE('',#11354);
#467=PLANE('',#11355);
#468=PLANE('',#11358);
#469=PLANE('',#11359);
#470=PLANE('',#11362);
#471=PLANE('',#11363);
#472=PLANE('',#11364);
#473=PLANE('',#11365);
#474=PLANE('',#11390);
#475=PLANE('',#11392);
#476=PLANE('',#11394);
#477=PLANE('',#11395);
#478=PLANE('',#11399);
#479=PLANE('',#11400);
#480=PLANE('',#11403);
#481=PLANE('',#11404);
#482=PLANE('',#11407);
#483=PLANE('',#11408);
#484=PLANE('',#11409);
#485=PLANE('',#11412);
#486=PLANE('',#11413);
#487=PLANE('',#11414);
#488=PLANE('',#11415);
#489=PLANE('',#11418);
#490=PLANE('',#11419);
#491=PLANE('',#11422);
#492=PLANE('',#11423);
#493=PLANE('',#11424);
#494=PLANE('',#11425);
#495=PLANE('',#11457);
#496=PLANE('',#11458);
#497=PLANE('',#11459);
#498=PLANE('',#11466);
#499=PLANE('',#11470);
#500=PLANE('',#11474);
#501=PLANE('',#11478);
#502=PLANE('',#11482);
#503=PLANE('',#11483);
#504=PLANE('',#11484);
#505=PLANE('',#11485);
#506=PLANE('',#11486);
#507=PLANE('',#11505);
#508=PLANE('',#11506);
#509=PLANE('',#11507);
#510=PLANE('',#11508);
#511=PLANE('',#11509);
#512=PLANE('',#11510);
#513=PLANE('',#11535);
#514=PLANE('',#11536);
#515=PLANE('',#11537);
#516=PLANE('',#11540);
#517=PLANE('',#11543);
#518=PLANE('',#11545);
#519=PLANE('',#11574);
#520=PLANE('',#11575);
#521=PLANE('',#11576);
#522=PLANE('',#11577);
#523=PLANE('',#11625);
#524=PLANE('',#11628);
#525=PLANE('',#11629);
#526=PLANE('',#11630);
#527=PLANE('',#11636);
#528=PLANE('',#11637);
#529=PLANE('',#11638);
#530=PLANE('',#11639);
#531=PLANE('',#11644);
#532=PLANE('',#11645);
#533=PLANE('',#11646);
#534=PLANE('',#11648);
#535=PLANE('',#11649);
#536=PLANE('',#11650);
#537=PLANE('',#11655);
#538=PLANE('',#11656);
#539=PLANE('',#11657);
#540=PLANE('',#11658);
#541=PLANE('',#11659);
#542=PLANE('',#11660);
#543=PLANE('',#11661);
#544=PLANE('',#11662);
#545=PLANE('',#11663);
#546=PLANE('',#11664);
#547=PLANE('',#11665);
#548=PLANE('',#11666);
#549=PLANE('',#11667);
#550=PLANE('',#11668);
#551=PLANE('',#11669);
#552=PLANE('',#11677);
#553=PLANE('',#11680);
#554=PLANE('',#11683);
#555=PLANE('',#11685);
#556=PLANE('',#11686);
#557=PLANE('',#11688);
#558=PLANE('',#11696);
#559=PLANE('',#11699);
#560=PLANE('',#11702);
#561=PLANE('',#11703);
#562=PLANE('',#11704);
#563=PLANE('',#11706);
#564=PLANE('',#11707);
#565=PLANE('',#11708);
#566=PLANE('',#11709);
#567=PLANE('',#11711);
#568=PLANE('',#11716);
#569=PLANE('',#11784);
#570=PLANE('',#11852);
#571=PLANE('',#11853);
#572=PLANE('',#11854);
#573=PLANE('',#11855);
#574=PLANE('',#11856);
#575=PLANE('',#11858);
#576=PLANE('',#11860);
#577=PLANE('',#11862);
#578=PLANE('',#11864);
#579=PLANE('',#11866);
#580=PLANE('',#11868);
#581=PLANE('',#11870);
#582=PLANE('',#11872);
#583=PLANE('',#11874);
#584=PLANE('',#11876);
#585=PLANE('',#11878);
#586=PLANE('',#11879);
#587=PLANE('',#11880);
#588=PLANE('',#11881);
#589=PLANE('',#11882);
#590=PLANE('',#11883);
#591=PLANE('',#11884);
#592=PLANE('',#11885);
#593=PLANE('',#11887);
#594=PLANE('',#11889);
#595=PLANE('',#11891);
#596=PLANE('',#11893);
#597=PLANE('',#11895);
#598=PLANE('',#11897);
#599=PLANE('',#11899);
#600=PLANE('',#11901);
#601=PLANE('',#11903);
#602=PLANE('',#11905);
#603=PLANE('',#11907);
#604=PLANE('',#11908);
#605=PLANE('',#11909);
#606=PLANE('',#11910);
#607=PLANE('',#11911);
#608=PLANE('',#11912);
#609=PLANE('',#11913);
#610=PLANE('',#11914);
#611=PLANE('',#11916);
#612=PLANE('',#11918);
#613=PLANE('',#11920);
#614=PLANE('',#11922);
#615=PLANE('',#11924);
#616=PLANE('',#11926);
#617=PLANE('',#11928);
#618=PLANE('',#11930);
#619=PLANE('',#11932);
#620=PLANE('',#11934);
#621=PLANE('',#11936);
#622=PLANE('',#11937);
#623=PLANE('',#11938);
#624=PLANE('',#11939);
#625=PLANE('',#11940);
#626=PLANE('',#11941);
#627=PLANE('',#11942);
#628=PLANE('',#11943);
#629=PLANE('',#11945);
#630=PLANE('',#11947);
#631=PLANE('',#11949);
#632=PLANE('',#11951);
#633=PLANE('',#11953);
#634=PLANE('',#11955);
#635=PLANE('',#11957);
#636=PLANE('',#11959);
#637=PLANE('',#11961);
#638=PLANE('',#11963);
#639=PLANE('',#11965);
#640=PLANE('',#11966);
#641=PLANE('',#11967);
#642=PLANE('',#11969);
#643=PLANE('',#11971);
#644=PLANE('',#11973);
#645=PLANE('',#11975);
#646=PLANE('',#11977);
#647=PLANE('',#11979);
#648=PLANE('',#11980);
#649=PLANE('',#11982);
#650=PLANE('',#11984);
#651=PLANE('',#11986);
#652=PLANE('',#11988);
#653=PLANE('',#11990);
#654=PLANE('',#11992);
#655=PLANE('',#11994);
#656=PLANE('',#11996);
#657=PLANE('',#11998);
#658=PLANE('',#12000);
#659=PLANE('',#12002);
#660=PLANE('',#12004);
#661=PLANE('',#12006);
#662=PLANE('',#12008);
#663=PLANE('',#12010);
#664=PLANE('',#12012);
#665=PLANE('',#12014);
#666=PLANE('',#12022);
#667=PLANE('',#12024);
#668=PLANE('',#12026);
#669=PLANE('',#12028);
#670=PLANE('',#12029);
#671=PLANE('',#12032);
#672=PLANE('',#12033);
#673=PLANE('',#12035);
#674=PLANE('',#12036);
#675=PLANE('',#12039);
#676=PLANE('',#12040);
#677=PLANE('',#12047);
#678=PLANE('',#12055);
#679=PLANE('',#12057);
#680=PLANE('',#12064);
#681=PLANE('',#12067);
#682=PLANE('',#12070);
#683=PLANE('',#12071);
#684=PLANE('',#12074);
#685=PLANE('',#12077);
#686=PLANE('',#12091);
#687=PLANE('',#12094);
#688=PLANE('',#12095);
#689=PLANE('',#12096);
#690=PLANE('',#12097);
#691=PLANE('',#12098);
#692=PLANE('',#12099);
#693=PLANE('',#12100);
#694=PLANE('',#12103);
#695=PLANE('',#12104);
#696=PLANE('',#12105);
#697=PLANE('',#12106);
#698=PLANE('',#12107);
#699=PLANE('',#12108);
#700=PLANE('',#12111);
#701=PLANE('',#12113);
#702=PLANE('',#12118);
#703=PLANE('',#12123);
#704=PLANE('',#12124);
#705=PLANE('',#12125);
#706=PLANE('',#12126);
#707=PLANE('',#12127);
#708=PLANE('',#12128);
#709=PLANE('',#12129);
#710=PLANE('',#12130);
#711=PLANE('',#12157);
#712=PLANE('',#12158);
#713=PLANE('',#12159);
#714=PLANE('',#12160);
#715=PLANE('',#12161);
#716=PLANE('',#12162);
#717=PLANE('',#12211);
#718=PLANE('',#12212);
#719=PLANE('',#12269);
#720=PLANE('',#12270);
#721=PLANE('',#12271);
#722=PLANE('',#12272);
#723=PLANE('',#12273);
#724=PLANE('',#12274);
#725=FACE_OUTER_BOUND('',#1321,.T.);
#726=FACE_OUTER_BOUND('',#1322,.T.);
#727=FACE_OUTER_BOUND('',#1323,.T.);
#728=FACE_OUTER_BOUND('',#1324,.T.);
#729=FACE_OUTER_BOUND('',#1325,.T.);
#730=FACE_OUTER_BOUND('',#1326,.T.);
#731=FACE_OUTER_BOUND('',#1327,.T.);
#732=FACE_OUTER_BOUND('',#1328,.T.);
#733=FACE_OUTER_BOUND('',#1329,.T.);
#734=FACE_OUTER_BOUND('',#1330,.T.);
#735=FACE_OUTER_BOUND('',#1331,.T.);
#736=FACE_OUTER_BOUND('',#1332,.T.);
#737=FACE_OUTER_BOUND('',#1333,.T.);
#738=FACE_OUTER_BOUND('',#1337,.T.);
#739=FACE_OUTER_BOUND('',#1338,.T.);
#740=FACE_OUTER_BOUND('',#1339,.T.);
#741=FACE_OUTER_BOUND('',#1340,.T.);
#742=FACE_OUTER_BOUND('',#1341,.T.);
#743=FACE_OUTER_BOUND('',#1342,.T.);
#744=FACE_OUTER_BOUND('',#1348,.T.);
#745=FACE_OUTER_BOUND('',#1350,.T.);
#746=FACE_OUTER_BOUND('',#1352,.T.);
#747=FACE_OUTER_BOUND('',#1353,.T.);
#748=FACE_OUTER_BOUND('',#1354,.T.);
#749=FACE_OUTER_BOUND('',#1355,.T.);
#750=FACE_OUTER_BOUND('',#1356,.T.);
#751=FACE_OUTER_BOUND('',#1357,.T.);
#752=FACE_OUTER_BOUND('',#1359,.T.);
#753=FACE_OUTER_BOUND('',#1361,.T.);
#754=FACE_OUTER_BOUND('',#1362,.T.);
#755=FACE_OUTER_BOUND('',#1363,.T.);
#756=FACE_OUTER_BOUND('',#1364,.T.);
#757=FACE_OUTER_BOUND('',#1365,.T.);
#758=FACE_OUTER_BOUND('',#1366,.T.);
#759=FACE_OUTER_BOUND('',#1367,.T.);
#760=FACE_OUTER_BOUND('',#1369,.T.);
#761=FACE_OUTER_BOUND('',#1370,.T.);
#762=FACE_OUTER_BOUND('',#1371,.T.);
#763=FACE_OUTER_BOUND('',#1372,.T.);
#764=FACE_OUTER_BOUND('',#1373,.T.);
#765=FACE_OUTER_BOUND('',#1374,.T.);
#766=FACE_OUTER_BOUND('',#1375,.T.);
#767=FACE_OUTER_BOUND('',#1377,.T.);
#768=FACE_OUTER_BOUND('',#1378,.T.);
#769=FACE_OUTER_BOUND('',#1379,.T.);
#770=FACE_OUTER_BOUND('',#1380,.T.);
#771=FACE_OUTER_BOUND('',#1383,.T.);
#772=FACE_OUTER_BOUND('',#1384,.T.);
#773=FACE_OUTER_BOUND('',#1385,.T.);
#774=FACE_OUTER_BOUND('',#1386,.T.);
#775=FACE_OUTER_BOUND('',#1387,.T.);
#776=FACE_OUTER_BOUND('',#1388,.T.);
#777=FACE_OUTER_BOUND('',#1389,.T.);
#778=FACE_OUTER_BOUND('',#1390,.T.);
#779=FACE_OUTER_BOUND('',#1391,.T.);
#780=FACE_OUTER_BOUND('',#1392,.T.);
#781=FACE_OUTER_BOUND('',#1393,.T.);
#782=FACE_OUTER_BOUND('',#1394,.T.);
#783=FACE_OUTER_BOUND('',#1395,.T.);
#784=FACE_OUTER_BOUND('',#1396,.T.);
#785=FACE_OUTER_BOUND('',#1397,.T.);
#786=FACE_OUTER_BOUND('',#1401,.T.);
#787=FACE_OUTER_BOUND('',#1402,.T.);
#788=FACE_OUTER_BOUND('',#1403,.T.);
#789=FACE_OUTER_BOUND('',#1404,.T.);
#790=FACE_OUTER_BOUND('',#1405,.T.);
#791=FACE_OUTER_BOUND('',#1406,.T.);
#792=FACE_OUTER_BOUND('',#1412,.T.);
#793=FACE_OUTER_BOUND('',#1414,.T.);
#794=FACE_OUTER_BOUND('',#1416,.T.);
#795=FACE_OUTER_BOUND('',#1417,.T.);
#796=FACE_OUTER_BOUND('',#1418,.T.);
#797=FACE_OUTER_BOUND('',#1419,.T.);
#798=FACE_OUTER_BOUND('',#1420,.T.);
#799=FACE_OUTER_BOUND('',#1421,.T.);
#800=FACE_OUTER_BOUND('',#1423,.T.);
#801=FACE_OUTER_BOUND('',#1425,.T.);
#802=FACE_OUTER_BOUND('',#1426,.T.);
#803=FACE_OUTER_BOUND('',#1427,.T.);
#804=FACE_OUTER_BOUND('',#1428,.T.);
#805=FACE_OUTER_BOUND('',#1429,.T.);
#806=FACE_OUTER_BOUND('',#1430,.T.);
#807=FACE_OUTER_BOUND('',#1431,.T.);
#808=FACE_OUTER_BOUND('',#1433,.T.);
#809=FACE_OUTER_BOUND('',#1434,.T.);
#810=FACE_OUTER_BOUND('',#1435,.T.);
#811=FACE_OUTER_BOUND('',#1436,.T.);
#812=FACE_OUTER_BOUND('',#1437,.T.);
#813=FACE_OUTER_BOUND('',#1438,.T.);
#814=FACE_OUTER_BOUND('',#1439,.T.);
#815=FACE_OUTER_BOUND('',#1441,.T.);
#816=FACE_OUTER_BOUND('',#1442,.T.);
#817=FACE_OUTER_BOUND('',#1443,.T.);
#818=FACE_OUTER_BOUND('',#1444,.T.);
#819=FACE_OUTER_BOUND('',#1447,.T.);
#820=FACE_OUTER_BOUND('',#1448,.T.);
#821=FACE_OUTER_BOUND('',#1449,.T.);
#822=FACE_OUTER_BOUND('',#1450,.T.);
#823=FACE_OUTER_BOUND('',#1451,.T.);
#824=FACE_OUTER_BOUND('',#1452,.T.);
#825=FACE_OUTER_BOUND('',#1453,.T.);
#826=FACE_OUTER_BOUND('',#1454,.T.);
#827=FACE_OUTER_BOUND('',#1455,.T.);
#828=FACE_OUTER_BOUND('',#1456,.T.);
#829=FACE_OUTER_BOUND('',#1457,.T.);
#830=FACE_OUTER_BOUND('',#1458,.T.);
#831=FACE_OUTER_BOUND('',#1459,.T.);
#832=FACE_OUTER_BOUND('',#1460,.T.);
#833=FACE_OUTER_BOUND('',#1461,.T.);
#834=FACE_OUTER_BOUND('',#1462,.T.);
#835=FACE_OUTER_BOUND('',#1463,.T.);
#836=FACE_OUTER_BOUND('',#1464,.T.);
#837=FACE_OUTER_BOUND('',#1467,.T.);
#838=FACE_OUTER_BOUND('',#1469,.T.);
#839=FACE_OUTER_BOUND('',#1471,.T.);
#840=FACE_OUTER_BOUND('',#1473,.T.);
#841=FACE_OUTER_BOUND('',#1474,.T.);
#842=FACE_OUTER_BOUND('',#1475,.T.);
#843=FACE_OUTER_BOUND('',#1477,.T.);
#844=FACE_OUTER_BOUND('',#1479,.T.);
#845=FACE_OUTER_BOUND('',#1480,.T.);
#846=FACE_OUTER_BOUND('',#1481,.T.);
#847=FACE_OUTER_BOUND('',#1482,.T.);
#848=FACE_OUTER_BOUND('',#1483,.T.);
#849=FACE_OUTER_BOUND('',#1484,.T.);
#850=FACE_OUTER_BOUND('',#1485,.T.);
#851=FACE_OUTER_BOUND('',#1486,.T.);
#852=FACE_OUTER_BOUND('',#1489,.T.);
#853=FACE_OUTER_BOUND('',#1490,.T.);
#854=FACE_OUTER_BOUND('',#1491,.T.);
#855=FACE_OUTER_BOUND('',#1492,.T.);
#856=FACE_OUTER_BOUND('',#1493,.T.);
#857=FACE_OUTER_BOUND('',#1494,.T.);
#858=FACE_OUTER_BOUND('',#1495,.T.);
#859=FACE_OUTER_BOUND('',#1496,.T.);
#860=FACE_OUTER_BOUND('',#1497,.T.);
#861=FACE_OUTER_BOUND('',#1498,.T.);
#862=FACE_OUTER_BOUND('',#1499,.T.);
#863=FACE_OUTER_BOUND('',#1500,.T.);
#864=FACE_OUTER_BOUND('',#1501,.T.);
#865=FACE_OUTER_BOUND('',#1502,.T.);
#866=FACE_OUTER_BOUND('',#1503,.T.);
#867=FACE_OUTER_BOUND('',#1504,.T.);
#868=FACE_OUTER_BOUND('',#1505,.T.);
#869=FACE_OUTER_BOUND('',#1506,.T.);
#870=FACE_OUTER_BOUND('',#1509,.T.);
#871=FACE_OUTER_BOUND('',#1511,.T.);
#872=FACE_OUTER_BOUND('',#1513,.T.);
#873=FACE_OUTER_BOUND('',#1515,.T.);
#874=FACE_OUTER_BOUND('',#1516,.T.);
#875=FACE_OUTER_BOUND('',#1517,.T.);
#876=FACE_OUTER_BOUND('',#1519,.T.);
#877=FACE_OUTER_BOUND('',#1521,.T.);
#878=FACE_OUTER_BOUND('',#1522,.T.);
#879=FACE_OUTER_BOUND('',#1523,.T.);
#880=FACE_OUTER_BOUND('',#1524,.T.);
#881=FACE_OUTER_BOUND('',#1525,.T.);
#882=FACE_OUTER_BOUND('',#1526,.T.);
#883=FACE_OUTER_BOUND('',#1527,.T.);
#884=FACE_OUTER_BOUND('',#1528,.T.);
#885=FACE_OUTER_BOUND('',#1531,.T.);
#886=FACE_OUTER_BOUND('',#1532,.T.);
#887=FACE_OUTER_BOUND('',#1533,.T.);
#888=FACE_OUTER_BOUND('',#1534,.T.);
#889=FACE_OUTER_BOUND('',#1535,.T.);
#890=FACE_OUTER_BOUND('',#1536,.T.);
#891=FACE_OUTER_BOUND('',#1537,.T.);
#892=FACE_OUTER_BOUND('',#1538,.T.);
#893=FACE_OUTER_BOUND('',#1539,.T.);
#894=FACE_OUTER_BOUND('',#1540,.T.);
#895=FACE_OUTER_BOUND('',#1541,.T.);
#896=FACE_OUTER_BOUND('',#1542,.T.);
#897=FACE_OUTER_BOUND('',#1543,.T.);
#898=FACE_OUTER_BOUND('',#1544,.T.);
#899=FACE_OUTER_BOUND('',#1545,.T.);
#900=FACE_OUTER_BOUND('',#1546,.T.);
#901=FACE_OUTER_BOUND('',#1547,.T.);
#902=FACE_OUTER_BOUND('',#1548,.T.);
#903=FACE_OUTER_BOUND('',#1549,.T.);
#904=FACE_OUTER_BOUND('',#1550,.T.);
#905=FACE_OUTER_BOUND('',#1551,.T.);
#906=FACE_OUTER_BOUND('',#1552,.T.);
#907=FACE_OUTER_BOUND('',#1553,.T.);
#908=FACE_OUTER_BOUND('',#1554,.T.);
#909=FACE_OUTER_BOUND('',#1555,.T.);
#910=FACE_OUTER_BOUND('',#1556,.T.);
#911=FACE_OUTER_BOUND('',#1557,.T.);
#912=FACE_OUTER_BOUND('',#1558,.T.);
#913=FACE_OUTER_BOUND('',#1559,.T.);
#914=FACE_OUTER_BOUND('',#1560,.T.);
#915=FACE_OUTER_BOUND('',#1561,.T.);
#916=FACE_OUTER_BOUND('',#1562,.T.);
#917=FACE_OUTER_BOUND('',#1563,.T.);
#918=FACE_OUTER_BOUND('',#1564,.T.);
#919=FACE_OUTER_BOUND('',#1565,.T.);
#920=FACE_OUTER_BOUND('',#1566,.T.);
#921=FACE_OUTER_BOUND('',#1567,.T.);
#922=FACE_OUTER_BOUND('',#1575,.T.);
#923=FACE_OUTER_BOUND('',#1577,.T.);
#924=FACE_OUTER_BOUND('',#1579,.T.);
#925=FACE_OUTER_BOUND('',#1587,.T.);
#926=FACE_OUTER_BOUND('',#1589,.T.);
#927=FACE_OUTER_BOUND('',#1591,.T.);
#928=FACE_OUTER_BOUND('',#1592,.T.);
#929=FACE_OUTER_BOUND('',#1593,.T.);
#930=FACE_OUTER_BOUND('',#1594,.T.);
#931=FACE_OUTER_BOUND('',#1595,.T.);
#932=FACE_OUTER_BOUND('',#1596,.T.);
#933=FACE_OUTER_BOUND('',#1597,.T.);
#934=FACE_OUTER_BOUND('',#1598,.T.);
#935=FACE_OUTER_BOUND('',#1600,.T.);
#936=FACE_OUTER_BOUND('',#1602,.T.);
#937=FACE_OUTER_BOUND('',#1604,.T.);
#938=FACE_OUTER_BOUND('',#1606,.T.);
#939=FACE_OUTER_BOUND('',#1607,.T.);
#940=FACE_OUTER_BOUND('',#1608,.T.);
#941=FACE_OUTER_BOUND('',#1609,.T.);
#942=FACE_OUTER_BOUND('',#1610,.T.);
#943=FACE_OUTER_BOUND('',#1611,.T.);
#944=FACE_OUTER_BOUND('',#1612,.T.);
#945=FACE_OUTER_BOUND('',#1613,.T.);
#946=FACE_OUTER_BOUND('',#1614,.T.);
#947=FACE_OUTER_BOUND('',#1615,.T.);
#948=FACE_OUTER_BOUND('',#1616,.T.);
#949=FACE_OUTER_BOUND('',#1617,.T.);
#950=FACE_OUTER_BOUND('',#1618,.T.);
#951=FACE_OUTER_BOUND('',#1620,.T.);
#952=FACE_OUTER_BOUND('',#1622,.T.);
#953=FACE_OUTER_BOUND('',#1624,.T.);
#954=FACE_OUTER_BOUND('',#1626,.T.);
#955=FACE_OUTER_BOUND('',#1627,.T.);
#956=FACE_OUTER_BOUND('',#1628,.T.);
#957=FACE_OUTER_BOUND('',#1629,.T.);
#958=FACE_OUTER_BOUND('',#1630,.T.);
#959=FACE_OUTER_BOUND('',#1631,.T.);
#960=FACE_OUTER_BOUND('',#1632,.T.);
#961=FACE_OUTER_BOUND('',#1633,.T.);
#962=FACE_OUTER_BOUND('',#1634,.T.);
#963=FACE_OUTER_BOUND('',#1635,.T.);
#964=FACE_OUTER_BOUND('',#1636,.T.);
#965=FACE_OUTER_BOUND('',#1637,.T.);
#966=FACE_OUTER_BOUND('',#1638,.T.);
#967=FACE_OUTER_BOUND('',#1645,.T.);
#968=FACE_OUTER_BOUND('',#1647,.T.);
#969=FACE_OUTER_BOUND('',#1648,.T.);
#970=FACE_OUTER_BOUND('',#1650,.T.);
#971=FACE_OUTER_BOUND('',#1651,.T.);
#972=FACE_OUTER_BOUND('',#1652,.T.);
#973=FACE_OUTER_BOUND('',#1653,.T.);
#974=FACE_OUTER_BOUND('',#1654,.T.);
#975=FACE_OUTER_BOUND('',#1655,.T.);
#976=FACE_OUTER_BOUND('',#1656,.T.);
#977=FACE_OUTER_BOUND('',#1657,.T.);
#978=FACE_OUTER_BOUND('',#1658,.T.);
#979=FACE_OUTER_BOUND('',#1664,.T.);
#980=FACE_OUTER_BOUND('',#1665,.T.);
#981=FACE_OUTER_BOUND('',#1666,.T.);
#982=FACE_OUTER_BOUND('',#1667,.T.);
#983=FACE_OUTER_BOUND('',#1668,.T.);
#984=FACE_OUTER_BOUND('',#1669,.T.);
#985=FACE_OUTER_BOUND('',#1670,.T.);
#986=FACE_OUTER_BOUND('',#1671,.T.);
#987=FACE_OUTER_BOUND('',#1672,.T.);
#988=FACE_OUTER_BOUND('',#1673,.T.);
#989=FACE_OUTER_BOUND('',#1674,.T.);
#990=FACE_OUTER_BOUND('',#1675,.T.);
#991=FACE_OUTER_BOUND('',#1676,.T.);
#992=FACE_OUTER_BOUND('',#1677,.T.);
#993=FACE_OUTER_BOUND('',#1678,.T.);
#994=FACE_OUTER_BOUND('',#1679,.T.);
#995=FACE_OUTER_BOUND('',#1680,.T.);
#996=FACE_OUTER_BOUND('',#1681,.T.);
#997=FACE_OUTER_BOUND('',#1683,.T.);
#998=FACE_OUTER_BOUND('',#1684,.T.);
#999=FACE_OUTER_BOUND('',#1686,.T.);
#1000=FACE_OUTER_BOUND('',#1687,.T.);
#1001=FACE_OUTER_BOUND('',#1688,.T.);
#1002=FACE_OUTER_BOUND('',#1689,.T.);
#1003=FACE_OUTER_BOUND('',#1690,.T.);
#1004=FACE_OUTER_BOUND('',#1691,.T.);
#1005=FACE_OUTER_BOUND('',#1693,.T.);
#1006=FACE_OUTER_BOUND('',#1695,.T.);
#1007=FACE_OUTER_BOUND('',#1696,.T.);
#1008=FACE_OUTER_BOUND('',#1697,.T.);
#1009=FACE_OUTER_BOUND('',#1698,.T.);
#1010=FACE_OUTER_BOUND('',#1699,.T.);
#1011=FACE_OUTER_BOUND('',#1700,.T.);
#1012=FACE_OUTER_BOUND('',#1701,.T.);
#1013=FACE_OUTER_BOUND('',#1702,.T.);
#1014=FACE_OUTER_BOUND('',#1703,.T.);
#1015=FACE_OUTER_BOUND('',#1705,.T.);
#1016=FACE_OUTER_BOUND('',#1707,.T.);
#1017=FACE_OUTER_BOUND('',#1708,.T.);
#1018=FACE_OUTER_BOUND('',#1709,.T.);
#1019=FACE_OUTER_BOUND('',#1710,.T.);
#1020=FACE_OUTER_BOUND('',#1711,.T.);
#1021=FACE_OUTER_BOUND('',#1712,.T.);
#1022=FACE_OUTER_BOUND('',#1713,.T.);
#1023=FACE_OUTER_BOUND('',#1714,.T.);
#1024=FACE_OUTER_BOUND('',#1715,.T.);
#1025=FACE_OUTER_BOUND('',#1716,.T.);
#1026=FACE_OUTER_BOUND('',#1717,.T.);
#1027=FACE_OUTER_BOUND('',#1718,.T.);
#1028=FACE_OUTER_BOUND('',#1724,.T.);
#1029=FACE_OUTER_BOUND('',#1730,.T.);
#1030=FACE_OUTER_BOUND('',#1731,.T.);
#1031=FACE_OUTER_BOUND('',#1732,.T.);
#1032=FACE_OUTER_BOUND('',#1733,.T.);
#1033=FACE_OUTER_BOUND('',#1734,.T.);
#1034=FACE_OUTER_BOUND('',#1735,.T.);
#1035=FACE_OUTER_BOUND('',#1736,.T.);
#1036=FACE_OUTER_BOUND('',#1737,.T.);
#1037=FACE_OUTER_BOUND('',#1738,.T.);
#1038=FACE_OUTER_BOUND('',#1739,.T.);
#1039=FACE_OUTER_BOUND('',#1740,.T.);
#1040=FACE_OUTER_BOUND('',#1741,.T.);
#1041=FACE_OUTER_BOUND('',#1742,.T.);
#1042=FACE_OUTER_BOUND('',#1743,.T.);
#1043=FACE_OUTER_BOUND('',#1744,.T.);
#1044=FACE_OUTER_BOUND('',#1745,.T.);
#1045=FACE_OUTER_BOUND('',#1746,.T.);
#1046=FACE_OUTER_BOUND('',#1747,.T.);
#1047=FACE_OUTER_BOUND('',#1748,.T.);
#1048=FACE_OUTER_BOUND('',#1749,.T.);
#1049=FACE_OUTER_BOUND('',#1750,.T.);
#1050=FACE_OUTER_BOUND('',#1751,.T.);
#1051=FACE_OUTER_BOUND('',#1752,.T.);
#1052=FACE_OUTER_BOUND('',#1753,.T.);
#1053=FACE_OUTER_BOUND('',#1754,.T.);
#1054=FACE_OUTER_BOUND('',#1755,.T.);
#1055=FACE_OUTER_BOUND('',#1756,.T.);
#1056=FACE_OUTER_BOUND('',#1757,.T.);
#1057=FACE_OUTER_BOUND('',#1758,.T.);
#1058=FACE_OUTER_BOUND('',#1759,.T.);
#1059=FACE_OUTER_BOUND('',#1760,.T.);
#1060=FACE_OUTER_BOUND('',#1761,.T.);
#1061=FACE_OUTER_BOUND('',#1762,.T.);
#1062=FACE_OUTER_BOUND('',#1763,.T.);
#1063=FACE_OUTER_BOUND('',#1764,.T.);
#1064=FACE_OUTER_BOUND('',#1765,.T.);
#1065=FACE_OUTER_BOUND('',#1766,.T.);
#1066=FACE_OUTER_BOUND('',#1767,.T.);
#1067=FACE_OUTER_BOUND('',#1768,.T.);
#1068=FACE_OUTER_BOUND('',#1769,.T.);
#1069=FACE_OUTER_BOUND('',#1770,.T.);
#1070=FACE_OUTER_BOUND('',#1771,.T.);
#1071=FACE_OUTER_BOUND('',#1772,.T.);
#1072=FACE_OUTER_BOUND('',#1773,.T.);
#1073=FACE_OUTER_BOUND('',#1774,.T.);
#1074=FACE_OUTER_BOUND('',#1775,.T.);
#1075=FACE_OUTER_BOUND('',#1776,.T.);
#1076=FACE_OUTER_BOUND('',#1777,.T.);
#1077=FACE_OUTER_BOUND('',#1778,.T.);
#1078=FACE_OUTER_BOUND('',#1779,.T.);
#1079=FACE_OUTER_BOUND('',#1780,.T.);
#1080=FACE_OUTER_BOUND('',#1781,.T.);
#1081=FACE_OUTER_BOUND('',#1782,.T.);
#1082=FACE_OUTER_BOUND('',#1783,.T.);
#1083=FACE_OUTER_BOUND('',#1784,.T.);
#1084=FACE_OUTER_BOUND('',#1785,.T.);
#1085=FACE_OUTER_BOUND('',#1786,.T.);
#1086=FACE_OUTER_BOUND('',#1787,.T.);
#1087=FACE_OUTER_BOUND('',#1788,.T.);
#1088=FACE_OUTER_BOUND('',#1789,.T.);
#1089=FACE_OUTER_BOUND('',#1790,.T.);
#1090=FACE_OUTER_BOUND('',#1791,.T.);
#1091=FACE_OUTER_BOUND('',#1792,.T.);
#1092=FACE_OUTER_BOUND('',#1793,.T.);
#1093=FACE_OUTER_BOUND('',#1794,.T.);
#1094=FACE_OUTER_BOUND('',#1795,.T.);
#1095=FACE_OUTER_BOUND('',#1796,.T.);
#1096=FACE_OUTER_BOUND('',#1797,.T.);
#1097=FACE_OUTER_BOUND('',#1798,.T.);
#1098=FACE_OUTER_BOUND('',#1799,.T.);
#1099=FACE_OUTER_BOUND('',#1800,.T.);
#1100=FACE_OUTER_BOUND('',#1801,.T.);
#1101=FACE_OUTER_BOUND('',#1802,.T.);
#1102=FACE_OUTER_BOUND('',#1803,.T.);
#1103=FACE_OUTER_BOUND('',#1804,.T.);
#1104=FACE_OUTER_BOUND('',#1805,.T.);
#1105=FACE_OUTER_BOUND('',#1806,.T.);
#1106=FACE_OUTER_BOUND('',#1807,.T.);
#1107=FACE_OUTER_BOUND('',#1808,.T.);
#1108=FACE_OUTER_BOUND('',#1809,.T.);
#1109=FACE_OUTER_BOUND('',#1810,.T.);
#1110=FACE_OUTER_BOUND('',#1811,.T.);
#1111=FACE_OUTER_BOUND('',#1812,.T.);
#1112=FACE_OUTER_BOUND('',#1813,.T.);
#1113=FACE_OUTER_BOUND('',#1814,.T.);
#1114=FACE_OUTER_BOUND('',#1815,.T.);
#1115=FACE_OUTER_BOUND('',#1816,.T.);
#1116=FACE_OUTER_BOUND('',#1817,.T.);
#1117=FACE_OUTER_BOUND('',#1818,.T.);
#1118=FACE_OUTER_BOUND('',#1819,.T.);
#1119=FACE_OUTER_BOUND('',#1820,.T.);
#1120=FACE_OUTER_BOUND('',#1821,.T.);
#1121=FACE_OUTER_BOUND('',#1822,.T.);
#1122=FACE_OUTER_BOUND('',#1823,.T.);
#1123=FACE_OUTER_BOUND('',#1824,.T.);
#1124=FACE_OUTER_BOUND('',#1825,.T.);
#1125=FACE_OUTER_BOUND('',#1826,.T.);
#1126=FACE_OUTER_BOUND('',#1827,.T.);
#1127=FACE_OUTER_BOUND('',#1828,.T.);
#1128=FACE_OUTER_BOUND('',#1829,.T.);
#1129=FACE_OUTER_BOUND('',#1830,.T.);
#1130=FACE_OUTER_BOUND('',#1831,.T.);
#1131=FACE_OUTER_BOUND('',#1832,.T.);
#1132=FACE_OUTER_BOUND('',#1833,.T.);
#1133=FACE_OUTER_BOUND('',#1834,.T.);
#1134=FACE_OUTER_BOUND('',#1835,.T.);
#1135=FACE_OUTER_BOUND('',#1836,.T.);
#1136=FACE_OUTER_BOUND('',#1837,.T.);
#1137=FACE_OUTER_BOUND('',#1838,.T.);
#1138=FACE_OUTER_BOUND('',#1839,.T.);
#1139=FACE_OUTER_BOUND('',#1840,.T.);
#1140=FACE_OUTER_BOUND('',#1841,.T.);
#1141=FACE_OUTER_BOUND('',#1842,.T.);
#1142=FACE_OUTER_BOUND('',#1843,.T.);
#1143=FACE_OUTER_BOUND('',#1844,.T.);
#1144=FACE_OUTER_BOUND('',#1845,.T.);
#1145=FACE_OUTER_BOUND('',#1846,.T.);
#1146=FACE_OUTER_BOUND('',#1847,.T.);
#1147=FACE_OUTER_BOUND('',#1848,.T.);
#1148=FACE_OUTER_BOUND('',#1849,.T.);
#1149=FACE_OUTER_BOUND('',#1850,.T.);
#1150=FACE_OUTER_BOUND('',#1851,.T.);
#1151=FACE_OUTER_BOUND('',#1852,.T.);
#1152=FACE_OUTER_BOUND('',#1853,.T.);
#1153=FACE_OUTER_BOUND('',#1854,.T.);
#1154=FACE_OUTER_BOUND('',#1855,.T.);
#1155=FACE_OUTER_BOUND('',#1856,.T.);
#1156=FACE_OUTER_BOUND('',#1857,.T.);
#1157=FACE_OUTER_BOUND('',#1858,.T.);
#1158=FACE_OUTER_BOUND('',#1859,.T.);
#1159=FACE_OUTER_BOUND('',#1860,.T.);
#1160=FACE_OUTER_BOUND('',#1861,.T.);
#1161=FACE_OUTER_BOUND('',#1862,.T.);
#1162=FACE_OUTER_BOUND('',#1863,.T.);
#1163=FACE_OUTER_BOUND('',#1864,.T.);
#1164=FACE_OUTER_BOUND('',#1865,.T.);
#1165=FACE_OUTER_BOUND('',#1866,.T.);
#1166=FACE_OUTER_BOUND('',#1867,.T.);
#1167=FACE_OUTER_BOUND('',#1868,.T.);
#1168=FACE_OUTER_BOUND('',#1869,.T.);
#1169=FACE_OUTER_BOUND('',#1870,.T.);
#1170=FACE_OUTER_BOUND('',#1871,.T.);
#1171=FACE_OUTER_BOUND('',#1872,.T.);
#1172=FACE_OUTER_BOUND('',#1873,.T.);
#1173=FACE_OUTER_BOUND('',#1874,.T.);
#1174=FACE_OUTER_BOUND('',#1875,.T.);
#1175=FACE_OUTER_BOUND('',#1876,.T.);
#1176=FACE_OUTER_BOUND('',#1877,.T.);
#1177=FACE_OUTER_BOUND('',#1878,.T.);
#1178=FACE_OUTER_BOUND('',#1879,.T.);
#1179=FACE_OUTER_BOUND('',#1880,.T.);
#1180=FACE_OUTER_BOUND('',#1881,.T.);
#1181=FACE_OUTER_BOUND('',#1882,.T.);
#1182=FACE_OUTER_BOUND('',#1883,.T.);
#1183=FACE_OUTER_BOUND('',#1884,.T.);
#1184=FACE_OUTER_BOUND('',#1885,.T.);
#1185=FACE_OUTER_BOUND('',#1886,.T.);
#1186=FACE_OUTER_BOUND('',#1887,.T.);
#1187=FACE_OUTER_BOUND('',#1888,.T.);
#1188=FACE_OUTER_BOUND('',#1889,.T.);
#1189=FACE_OUTER_BOUND('',#1890,.T.);
#1190=FACE_OUTER_BOUND('',#1891,.T.);
#1191=FACE_OUTER_BOUND('',#1892,.T.);
#1192=FACE_OUTER_BOUND('',#1893,.T.);
#1193=FACE_OUTER_BOUND('',#1894,.T.);
#1194=FACE_OUTER_BOUND('',#1895,.T.);
#1195=FACE_OUTER_BOUND('',#1896,.T.);
#1196=FACE_OUTER_BOUND('',#1897,.T.);
#1197=FACE_OUTER_BOUND('',#1898,.T.);
#1198=FACE_OUTER_BOUND('',#1899,.T.);
#1199=FACE_OUTER_BOUND('',#1901,.T.);
#1200=FACE_OUTER_BOUND('',#1902,.T.);
#1201=FACE_OUTER_BOUND('',#1903,.T.);
#1202=FACE_OUTER_BOUND('',#1904,.T.);
#1203=FACE_OUTER_BOUND('',#1906,.T.);
#1204=FACE_OUTER_BOUND('',#1907,.T.);
#1205=FACE_OUTER_BOUND('',#1909,.T.);
#1206=FACE_OUTER_BOUND('',#1911,.T.);
#1207=FACE_OUTER_BOUND('',#1912,.T.);
#1208=FACE_OUTER_BOUND('',#1913,.T.);
#1209=FACE_OUTER_BOUND('',#1914,.T.);
#1210=FACE_OUTER_BOUND('',#1915,.T.);
#1211=FACE_OUTER_BOUND('',#1916,.T.);
#1212=FACE_OUTER_BOUND('',#1917,.T.);
#1213=FACE_OUTER_BOUND('',#1918,.T.);
#1214=FACE_OUTER_BOUND('',#1919,.T.);
#1215=FACE_OUTER_BOUND('',#1920,.T.);
#1216=FACE_OUTER_BOUND('',#1921,.T.);
#1217=FACE_OUTER_BOUND('',#1922,.T.);
#1218=FACE_OUTER_BOUND('',#1923,.T.);
#1219=FACE_OUTER_BOUND('',#1925,.T.);
#1220=FACE_OUTER_BOUND('',#1926,.T.);
#1221=FACE_OUTER_BOUND('',#1927,.T.);
#1222=FACE_OUTER_BOUND('',#1929,.T.);
#1223=FACE_OUTER_BOUND('',#1930,.T.);
#1224=FACE_OUTER_BOUND('',#1931,.T.);
#1225=FACE_OUTER_BOUND('',#1932,.T.);
#1226=FACE_OUTER_BOUND('',#1933,.T.);
#1227=FACE_OUTER_BOUND('',#1934,.T.);
#1228=FACE_OUTER_BOUND('',#1935,.T.);
#1229=FACE_OUTER_BOUND('',#1936,.T.);
#1230=FACE_OUTER_BOUND('',#1937,.T.);
#1231=FACE_OUTER_BOUND('',#1938,.T.);
#1232=FACE_OUTER_BOUND('',#1939,.T.);
#1233=FACE_OUTER_BOUND('',#1940,.T.);
#1234=FACE_OUTER_BOUND('',#1941,.T.);
#1235=FACE_OUTER_BOUND('',#1942,.T.);
#1236=FACE_OUTER_BOUND('',#1943,.T.);
#1237=FACE_OUTER_BOUND('',#1944,.T.);
#1238=FACE_OUTER_BOUND('',#1946,.T.);
#1239=FACE_OUTER_BOUND('',#1947,.T.);
#1240=FACE_OUTER_BOUND('',#1948,.T.);
#1241=FACE_OUTER_BOUND('',#1949,.T.);
#1242=FACE_OUTER_BOUND('',#1950,.T.);
#1243=FACE_OUTER_BOUND('',#1951,.T.);
#1244=FACE_OUTER_BOUND('',#1953,.T.);
#1245=FACE_OUTER_BOUND('',#1954,.T.);
#1246=FACE_OUTER_BOUND('',#1955,.T.);
#1247=FACE_OUTER_BOUND('',#1957,.T.);
#1248=FACE_OUTER_BOUND('',#1959,.T.);
#1249=FACE_OUTER_BOUND('',#1961,.T.);
#1250=FACE_OUTER_BOUND('',#1962,.T.);
#1251=FACE_OUTER_BOUND('',#1963,.T.);
#1252=FACE_OUTER_BOUND('',#1964,.T.);
#1253=FACE_OUTER_BOUND('',#1965,.T.);
#1254=FACE_OUTER_BOUND('',#1966,.T.);
#1255=FACE_OUTER_BOUND('',#1967,.T.);
#1256=FACE_OUTER_BOUND('',#1968,.T.);
#1257=FACE_OUTER_BOUND('',#1969,.T.);
#1258=FACE_OUTER_BOUND('',#1970,.T.);
#1259=FACE_OUTER_BOUND('',#1971,.T.);
#1260=FACE_OUTER_BOUND('',#1972,.T.);
#1261=FACE_OUTER_BOUND('',#1973,.T.);
#1262=FACE_OUTER_BOUND('',#1974,.T.);
#1263=FACE_OUTER_BOUND('',#1975,.T.);
#1264=FACE_OUTER_BOUND('',#1976,.T.);
#1265=FACE_OUTER_BOUND('',#1977,.T.);
#1266=FACE_OUTER_BOUND('',#1978,.T.);
#1267=FACE_OUTER_BOUND('',#1979,.T.);
#1268=FACE_OUTER_BOUND('',#1980,.T.);
#1269=FACE_OUTER_BOUND('',#1982,.T.);
#1270=FACE_OUTER_BOUND('',#1984,.T.);
#1271=FACE_OUTER_BOUND('',#1986,.T.);
#1272=FACE_OUTER_BOUND('',#1988,.T.);
#1273=FACE_OUTER_BOUND('',#1990,.T.);
#1274=FACE_OUTER_BOUND('',#1992,.T.);
#1275=FACE_OUTER_BOUND('',#1993,.T.);
#1276=FACE_OUTER_BOUND('',#1994,.T.);
#1277=FACE_OUTER_BOUND('',#1995,.T.);
#1278=FACE_OUTER_BOUND('',#1996,.T.);
#1279=FACE_OUTER_BOUND('',#1997,.T.);
#1280=FACE_OUTER_BOUND('',#1998,.T.);
#1281=FACE_OUTER_BOUND('',#1999,.T.);
#1282=FACE_OUTER_BOUND('',#2000,.T.);
#1283=FACE_OUTER_BOUND('',#2001,.T.);
#1284=FACE_OUTER_BOUND('',#2002,.T.);
#1285=FACE_OUTER_BOUND('',#2003,.T.);
#1286=FACE_OUTER_BOUND('',#2004,.T.);
#1287=FACE_OUTER_BOUND('',#2005,.T.);
#1288=FACE_OUTER_BOUND('',#2006,.T.);
#1289=FACE_OUTER_BOUND('',#2007,.T.);
#1290=FACE_OUTER_BOUND('',#2008,.T.);
#1291=FACE_OUTER_BOUND('',#2009,.T.);
#1292=FACE_OUTER_BOUND('',#2010,.T.);
#1293=FACE_OUTER_BOUND('',#2011,.T.);
#1294=FACE_OUTER_BOUND('',#2013,.T.);
#1295=FACE_OUTER_BOUND('',#2015,.T.);
#1296=FACE_OUTER_BOUND('',#2016,.T.);
#1297=FACE_OUTER_BOUND('',#2017,.T.);
#1298=FACE_OUTER_BOUND('',#2018,.T.);
#1299=FACE_OUTER_BOUND('',#2019,.T.);
#1300=FACE_OUTER_BOUND('',#2020,.T.);
#1301=FACE_OUTER_BOUND('',#2021,.T.);
#1302=FACE_OUTER_BOUND('',#2022,.T.);
#1303=FACE_OUTER_BOUND('',#2023,.T.);
#1304=FACE_OUTER_BOUND('',#2024,.T.);
#1305=FACE_OUTER_BOUND('',#2025,.T.);
#1306=FACE_OUTER_BOUND('',#2026,.T.);
#1307=FACE_OUTER_BOUND('',#2027,.T.);
#1308=FACE_OUTER_BOUND('',#2028,.T.);
#1309=FACE_OUTER_BOUND('',#2029,.T.);
#1310=FACE_OUTER_BOUND('',#2030,.T.);
#1311=FACE_OUTER_BOUND('',#2031,.T.);
#1312=FACE_OUTER_BOUND('',#2032,.T.);
#1313=FACE_OUTER_BOUND('',#2033,.T.);
#1314=FACE_OUTER_BOUND('',#2034,.T.);
#1315=FACE_OUTER_BOUND('',#2035,.T.);
#1316=FACE_OUTER_BOUND('',#2037,.T.);
#1317=FACE_OUTER_BOUND('',#2039,.T.);
#1318=FACE_OUTER_BOUND('',#2041,.T.);
#1319=FACE_OUTER_BOUND('',#2043,.T.);
#1320=FACE_OUTER_BOUND('',#2045,.T.);
#1321=EDGE_LOOP('',(#7108,#7109,#7110,#7111));
#1322=EDGE_LOOP('',(#7112,#7113,#7114,#7115));
#1323=EDGE_LOOP('',(#7116,#7117,#7118,#7119));
#1324=EDGE_LOOP('',(#7120,#7121,#7122,#7123));
#1325=EDGE_LOOP('',(#7124,#7125,#7126,#7127));
#1326=EDGE_LOOP('',(#7128,#7129,#7130,#7131));
#1327=EDGE_LOOP('',(#7132,#7133,#7134,#7135));
#1328=EDGE_LOOP('',(#7136,#7137,#7138,#7139));
#1329=EDGE_LOOP('',(#7140,#7141,#7142,#7143));
#1330=EDGE_LOOP('',(#7144,#7145,#7146,#7147,#7148,#7149,#7150,#7151,#7152,
#7153));
#1331=EDGE_LOOP('',(#7154,#7155,#7156,#7157,#7158));
#1332=EDGE_LOOP('',(#7159,#7160,#7161,#7162,#7163));
#1333=EDGE_LOOP('',(#7164,#7165,#7166,#7167,#7168,#7169,#7170,#7171,#7172));
#1334=EDGE_LOOP('',(#7173,#7174,#7175,#7176,#7177,#7178));
#1335=EDGE_LOOP('',(#7179,#7180,#7181,#7182,#7183,#7184));
#1336=EDGE_LOOP('',(#7185));
#1337=EDGE_LOOP('',(#7186,#7187,#7188,#7189,#7190));
#1338=EDGE_LOOP('',(#7191,#7192,#7193,#7194));
#1339=EDGE_LOOP('',(#7195,#7196,#7197,#7198,#7199,#7200,#7201,#7202));
#1340=EDGE_LOOP('',(#7203,#7204,#7205,#7206,#7207,#7208,#7209,#7210));
#1341=EDGE_LOOP('',(#7211,#7212,#7213,#7214));
#1342=EDGE_LOOP('',(#7215,#7216,#7217,#7218,#7219,#7220,#7221));
#1343=EDGE_LOOP('',(#7222));
#1344=EDGE_LOOP('',(#7223));
#1345=EDGE_LOOP('',(#7224));
#1346=EDGE_LOOP('',(#7225));
#1347=EDGE_LOOP('',(#7226));
#1348=EDGE_LOOP('',(#7227));
#1349=EDGE_LOOP('',(#7228));
#1350=EDGE_LOOP('',(#7229));
#1351=EDGE_LOOP('',(#7230));
#1352=EDGE_LOOP('',(#7231,#7232,#7233,#7234));
#1353=EDGE_LOOP('',(#7235,#7236,#7237,#7238));
#1354=EDGE_LOOP('',(#7239,#7240,#7241,#7242,#7243,#7244,#7245));
#1355=EDGE_LOOP('',(#7246,#7247,#7248,#7249));
#1356=EDGE_LOOP('',(#7250,#7251,#7252,#7253));
#1357=EDGE_LOOP('',(#7254));
#1358=EDGE_LOOP('',(#7255));
#1359=EDGE_LOOP('',(#7256));
#1360=EDGE_LOOP('',(#7257));
#1361=EDGE_LOOP('',(#7258,#7259,#7260,#7261));
#1362=EDGE_LOOP('',(#7262,#7263,#7264,#7265));
#1363=EDGE_LOOP('',(#7266,#7267,#7268,#7269));
#1364=EDGE_LOOP('',(#7270,#7271,#7272,#7273));
#1365=EDGE_LOOP('',(#7274,#7275,#7276,#7277));
#1366=EDGE_LOOP('',(#7278,#7279,#7280,#7281));
#1367=EDGE_LOOP('',(#7282,#7283,#7284,#7285,#7286,#7287));
#1368=EDGE_LOOP('',(#7288));
#1369=EDGE_LOOP('',(#7289,#7290,#7291,#7292));
#1370=EDGE_LOOP('',(#7293,#7294,#7295,#7296));
#1371=EDGE_LOOP('',(#7297,#7298,#7299,#7300));
#1372=EDGE_LOOP('',(#7301,#7302,#7303,#7304));
#1373=EDGE_LOOP('',(#7305,#7306,#7307,#7308));
#1374=EDGE_LOOP('',(#7309,#7310,#7311,#7312));
#1375=EDGE_LOOP('',(#7313,#7314,#7315,#7316,#7317,#7318));
#1376=EDGE_LOOP('',(#7319));
#1377=EDGE_LOOP('',(#7320,#7321,#7322,#7323));
#1378=EDGE_LOOP('',(#7324,#7325,#7326,#7327));
#1379=EDGE_LOOP('',(#7328,#7329,#7330,#7331));
#1380=EDGE_LOOP('',(#7332,#7333,#7334,#7335));
#1381=EDGE_LOOP('',(#7336));
#1382=EDGE_LOOP('',(#7337));
#1383=EDGE_LOOP('',(#7338,#7339,#7340,#7341));
#1384=EDGE_LOOP('',(#7342,#7343,#7344,#7345));
#1385=EDGE_LOOP('',(#7346,#7347,#7348,#7349));
#1386=EDGE_LOOP('',(#7350,#7351,#7352,#7353));
#1387=EDGE_LOOP('',(#7354,#7355,#7356,#7357));
#1388=EDGE_LOOP('',(#7358,#7359,#7360,#7361));
#1389=EDGE_LOOP('',(#7362,#7363,#7364,#7365));
#1390=EDGE_LOOP('',(#7366,#7367,#7368,#7369));
#1391=EDGE_LOOP('',(#7370,#7371,#7372,#7373));
#1392=EDGE_LOOP('',(#7374,#7375,#7376,#7377));
#1393=EDGE_LOOP('',(#7378,#7379,#7380,#7381));
#1394=EDGE_LOOP('',(#7382,#7383,#7384,#7385,#7386,#7387,#7388,#7389,#7390,
#7391));
#1395=EDGE_LOOP('',(#7392,#7393,#7394,#7395,#7396));
#1396=EDGE_LOOP('',(#7397,#7398,#7399,#7400,#7401));
#1397=EDGE_LOOP('',(#7402,#7403,#7404,#7405,#7406,#7407,#7408,#7409,#7410));
#1398=EDGE_LOOP('',(#7411,#7412,#7413,#7414,#7415,#7416));
#1399=EDGE_LOOP('',(#7417,#7418,#7419,#7420,#7421,#7422));
#1400=EDGE_LOOP('',(#7423));
#1401=EDGE_LOOP('',(#7424,#7425,#7426,#7427,#7428));
#1402=EDGE_LOOP('',(#7429,#7430,#7431,#7432));
#1403=EDGE_LOOP('',(#7433,#7434,#7435,#7436,#7437,#7438,#7439,#7440));
#1404=EDGE_LOOP('',(#7441,#7442,#7443,#7444,#7445,#7446,#7447,#7448));
#1405=EDGE_LOOP('',(#7449,#7450,#7451,#7452));
#1406=EDGE_LOOP('',(#7453,#7454,#7455,#7456,#7457,#7458,#7459));
#1407=EDGE_LOOP('',(#7460));
#1408=EDGE_LOOP('',(#7461));
#1409=EDGE_LOOP('',(#7462));
#1410=EDGE_LOOP('',(#7463));
#1411=EDGE_LOOP('',(#7464));
#1412=EDGE_LOOP('',(#7465));
#1413=EDGE_LOOP('',(#7466));
#1414=EDGE_LOOP('',(#7467));
#1415=EDGE_LOOP('',(#7468));
#1416=EDGE_LOOP('',(#7469,#7470,#7471,#7472));
#1417=EDGE_LOOP('',(#7473,#7474,#7475,#7476));
#1418=EDGE_LOOP('',(#7477,#7478,#7479,#7480,#7481,#7482,#7483));
#1419=EDGE_LOOP('',(#7484,#7485,#7486,#7487));
#1420=EDGE_LOOP('',(#7488,#7489,#7490,#7491));
#1421=EDGE_LOOP('',(#7492));
#1422=EDGE_LOOP('',(#7493));
#1423=EDGE_LOOP('',(#7494));
#1424=EDGE_LOOP('',(#7495));
#1425=EDGE_LOOP('',(#7496,#7497,#7498,#7499));
#1426=EDGE_LOOP('',(#7500,#7501,#7502,#7503));
#1427=EDGE_LOOP('',(#7504,#7505,#7506,#7507));
#1428=EDGE_LOOP('',(#7508,#7509,#7510,#7511));
#1429=EDGE_LOOP('',(#7512,#7513,#7514,#7515));
#1430=EDGE_LOOP('',(#7516,#7517,#7518,#7519));
#1431=EDGE_LOOP('',(#7520,#7521,#7522,#7523,#7524,#7525));
#1432=EDGE_LOOP('',(#7526));
#1433=EDGE_LOOP('',(#7527,#7528,#7529,#7530));
#1434=EDGE_LOOP('',(#7531,#7532,#7533,#7534));
#1435=EDGE_LOOP('',(#7535,#7536,#7537,#7538));
#1436=EDGE_LOOP('',(#7539,#7540,#7541,#7542));
#1437=EDGE_LOOP('',(#7543,#7544,#7545,#7546));
#1438=EDGE_LOOP('',(#7547,#7548,#7549,#7550));
#1439=EDGE_LOOP('',(#7551,#7552,#7553,#7554,#7555,#7556));
#1440=EDGE_LOOP('',(#7557));
#1441=EDGE_LOOP('',(#7558,#7559,#7560,#7561));
#1442=EDGE_LOOP('',(#7562,#7563,#7564,#7565));
#1443=EDGE_LOOP('',(#7566,#7567,#7568,#7569));
#1444=EDGE_LOOP('',(#7570,#7571,#7572,#7573));
#1445=EDGE_LOOP('',(#7574));
#1446=EDGE_LOOP('',(#7575));
#1447=EDGE_LOOP('',(#7576,#7577,#7578,#7579));
#1448=EDGE_LOOP('',(#7580,#7581,#7582,#7583));
#1449=EDGE_LOOP('',(#7584,#7585,#7586,#7587,#7588,#7589));
#1450=EDGE_LOOP('',(#7590,#7591,#7592,#7593));
#1451=EDGE_LOOP('',(#7594,#7595,#7596,#7597));
#1452=EDGE_LOOP('',(#7598,#7599,#7600,#7601));
#1453=EDGE_LOOP('',(#7602,#7603,#7604,#7605));
#1454=EDGE_LOOP('',(#7606,#7607,#7608,#7609));
#1455=EDGE_LOOP('',(#7610,#7611,#7612,#7613));
#1456=EDGE_LOOP('',(#7614,#7615,#7616,#7617,#7618));
#1457=EDGE_LOOP('',(#7619,#7620,#7621,#7622,#7623));
#1458=EDGE_LOOP('',(#7624,#7625,#7626,#7627,#7628,#7629,#7630,#7631));
#1459=EDGE_LOOP('',(#7632,#7633,#7634,#7635,#7636));
#1460=EDGE_LOOP('',(#7637,#7638,#7639,#7640));
#1461=EDGE_LOOP('',(#7641,#7642,#7643,#7644,#7645,#7646));
#1462=EDGE_LOOP('',(#7647,#7648,#7649,#7650,#7651,#7652,#7653,#7654,#7655,
#7656,#7657,#7658,#7659,#7660));
#1463=EDGE_LOOP('',(#7661,#7662,#7663,#7664));
#1464=EDGE_LOOP('',(#7665,#7666,#7667,#7668,#7669,#7670,#7671,#7672,#7673,
#7674,#7675,#7676,#7677));
#1465=EDGE_LOOP('',(#7678));
#1466=EDGE_LOOP('',(#7679));
#1467=EDGE_LOOP('',(#7680,#7681,#7682,#7683));
#1468=EDGE_LOOP('',(#7684));
#1469=EDGE_LOOP('',(#7685));
#1470=EDGE_LOOP('',(#7686));
#1471=EDGE_LOOP('',(#7687));
#1472=EDGE_LOOP('',(#7688));
#1473=EDGE_LOOP('',(#7689,#7690,#7691,#7692));
#1474=EDGE_LOOP('',(#7693,#7694,#7695,#7696));
#1475=EDGE_LOOP('',(#7697));
#1476=EDGE_LOOP('',(#7698));
#1477=EDGE_LOOP('',(#7699));
#1478=EDGE_LOOP('',(#7700));
#1479=EDGE_LOOP('',(#7701,#7702,#7703,#7704,#7705));
#1480=EDGE_LOOP('',(#7706,#7707,#7708,#7709,#7710,#7711));
#1481=EDGE_LOOP('',(#7712,#7713,#7714,#7715,#7716));
#1482=EDGE_LOOP('',(#7717,#7718,#7719,#7720));
#1483=EDGE_LOOP('',(#7721,#7722,#7723,#7724));
#1484=EDGE_LOOP('',(#7725,#7726,#7727,#7728));
#1485=EDGE_LOOP('',(#7729,#7730,#7731,#7732,#7733,#7734,#7735));
#1486=EDGE_LOOP('',(#7736,#7737,#7738,#7739));
#1487=EDGE_LOOP('',(#7740));
#1488=EDGE_LOOP('',(#7741));
#1489=EDGE_LOOP('',(#7742,#7743,#7744,#7745));
#1490=EDGE_LOOP('',(#7746,#7747,#7748,#7749));
#1491=EDGE_LOOP('',(#7750,#7751,#7752,#7753,#7754,#7755));
#1492=EDGE_LOOP('',(#7756,#7757,#7758,#7759));
#1493=EDGE_LOOP('',(#7760,#7761,#7762,#7763));
#1494=EDGE_LOOP('',(#7764,#7765,#7766,#7767));
#1495=EDGE_LOOP('',(#7768,#7769,#7770,#7771));
#1496=EDGE_LOOP('',(#7772,#7773,#7774,#7775));
#1497=EDGE_LOOP('',(#7776,#7777,#7778,#7779));
#1498=EDGE_LOOP('',(#7780,#7781,#7782,#7783,#7784));
#1499=EDGE_LOOP('',(#7785,#7786,#7787,#7788,#7789));
#1500=EDGE_LOOP('',(#7790,#7791,#7792,#7793,#7794,#7795,#7796,#7797));
#1501=EDGE_LOOP('',(#7798,#7799,#7800,#7801,#7802));
#1502=EDGE_LOOP('',(#7803,#7804,#7805,#7806));
#1503=EDGE_LOOP('',(#7807,#7808,#7809,#7810,#7811,#7812));
#1504=EDGE_LOOP('',(#7813,#7814,#7815,#7816,#7817,#7818,#7819,#7820,#7821,
#7822,#7823,#7824,#7825,#7826));
#1505=EDGE_LOOP('',(#7827,#7828,#7829,#7830));
#1506=EDGE_LOOP('',(#7831,#7832,#7833,#7834,#7835,#7836,#7837,#7838,#7839,
#7840,#7841,#7842,#7843));
#1507=EDGE_LOOP('',(#7844));
#1508=EDGE_LOOP('',(#7845));
#1509=EDGE_LOOP('',(#7846,#7847,#7848,#7849));
#1510=EDGE_LOOP('',(#7850));
#1511=EDGE_LOOP('',(#7851));
#1512=EDGE_LOOP('',(#7852));
#1513=EDGE_LOOP('',(#7853));
#1514=EDGE_LOOP('',(#7854));
#1515=EDGE_LOOP('',(#7855,#7856,#7857,#7858));
#1516=EDGE_LOOP('',(#7859,#7860,#7861,#7862));
#1517=EDGE_LOOP('',(#7863));
#1518=EDGE_LOOP('',(#7864));
#1519=EDGE_LOOP('',(#7865));
#1520=EDGE_LOOP('',(#7866));
#1521=EDGE_LOOP('',(#7867,#7868,#7869,#7870,#7871));
#1522=EDGE_LOOP('',(#7872,#7873,#7874,#7875,#7876,#7877));
#1523=EDGE_LOOP('',(#7878,#7879,#7880,#7881,#7882));
#1524=EDGE_LOOP('',(#7883,#7884,#7885,#7886));
#1525=EDGE_LOOP('',(#7887,#7888,#7889,#7890));
#1526=EDGE_LOOP('',(#7891,#7892,#7893,#7894));
#1527=EDGE_LOOP('',(#7895,#7896,#7897,#7898,#7899,#7900,#7901));
#1528=EDGE_LOOP('',(#7902,#7903,#7904,#7905));
#1529=EDGE_LOOP('',(#7906));
#1530=EDGE_LOOP('',(#7907));
#1531=EDGE_LOOP('',(#7908,#7909,#7910,#7911));
#1532=EDGE_LOOP('',(#7912,#7913,#7914,#7915));
#1533=EDGE_LOOP('',(#7916,#7917,#7918,#7919));
#1534=EDGE_LOOP('',(#7920,#7921,#7922,#7923));
#1535=EDGE_LOOP('',(#7924,#7925,#7926,#7927));
#1536=EDGE_LOOP('',(#7928,#7929,#7930,#7931));
#1537=EDGE_LOOP('',(#7932,#7933,#7934,#7935));
#1538=EDGE_LOOP('',(#7936,#7937,#7938,#7939));
#1539=EDGE_LOOP('',(#7940,#7941,#7942,#7943));
#1540=EDGE_LOOP('',(#7944,#7945,#7946,#7947));
#1541=EDGE_LOOP('',(#7948,#7949,#7950,#7951));
#1542=EDGE_LOOP('',(#7952,#7953,#7954,#7955));
#1543=EDGE_LOOP('',(#7956,#7957,#7958,#7959));
#1544=EDGE_LOOP('',(#7960,#7961,#7962,#7963));
#1545=EDGE_LOOP('',(#7964,#7965,#7966,#7967));
#1546=EDGE_LOOP('',(#7968,#7969,#7970,#7971));
#1547=EDGE_LOOP('',(#7972,#7973,#7974,#7975));
#1548=EDGE_LOOP('',(#7976,#7977,#7978,#7979));
#1549=EDGE_LOOP('',(#7980,#7981,#7982,#7983));
#1550=EDGE_LOOP('',(#7984,#7985,#7986,#7987));
#1551=EDGE_LOOP('',(#7988,#7989,#7990,#7991));
#1552=EDGE_LOOP('',(#7992,#7993,#7994,#7995));
#1553=EDGE_LOOP('',(#7996,#7997,#7998,#7999));
#1554=EDGE_LOOP('',(#8000,#8001,#8002,#8003));
#1555=EDGE_LOOP('',(#8004,#8005,#8006,#8007));
#1556=EDGE_LOOP('',(#8008,#8009,#8010,#8011));
#1557=EDGE_LOOP('',(#8012,#8013,#8014,#8015));
#1558=EDGE_LOOP('',(#8016,#8017,#8018,#8019));
#1559=EDGE_LOOP('',(#8020,#8021,#8022,#8023));
#1560=EDGE_LOOP('',(#8024,#8025,#8026,#8027));
#1561=EDGE_LOOP('',(#8028,#8029,#8030,#8031));
#1562=EDGE_LOOP('',(#8032,#8033,#8034,#8035));
#1563=EDGE_LOOP('',(#8036,#8037,#8038,#8039));
#1564=EDGE_LOOP('',(#8040,#8041,#8042,#8043));
#1565=EDGE_LOOP('',(#8044,#8045,#8046,#8047));
#1566=EDGE_LOOP('',(#8048,#8049,#8050,#8051));
#1567=EDGE_LOOP('',(#8052,#8053,#8054,#8055,#8056,#8057,#8058,#8059,#8060,
#8061,#8062,#8063,#8064,#8065,#8066,#8067));
#1568=EDGE_LOOP('',(#8068,#8069,#8070,#8071,#8072,#8073,#8074,#8075));
#1569=EDGE_LOOP('',(#8076));
#1570=EDGE_LOOP('',(#8077));
#1571=EDGE_LOOP('',(#8078));
#1572=EDGE_LOOP('',(#8079));
#1573=EDGE_LOOP('',(#8080));
#1574=EDGE_LOOP('',(#8081));
#1575=EDGE_LOOP('',(#8082));
#1576=EDGE_LOOP('',(#8083));
#1577=EDGE_LOOP('',(#8084));
#1578=EDGE_LOOP('',(#8085));
#1579=EDGE_LOOP('',(#8086,#8087,#8088,#8089,#8090,#8091,#8092,#8093,#8094,
#8095,#8096,#8097,#8098,#8099,#8100,#8101));
#1580=EDGE_LOOP('',(#8102));
#1581=EDGE_LOOP('',(#8103));
#1582=EDGE_LOOP('',(#8104));
#1583=EDGE_LOOP('',(#8105));
#1584=EDGE_LOOP('',(#8106));
#1585=EDGE_LOOP('',(#8107));
#1586=EDGE_LOOP('',(#8108,#8109,#8110,#8111,#8112,#8113,#8114,#8115));
#1587=EDGE_LOOP('',(#8116));
#1588=EDGE_LOOP('',(#8117));
#1589=EDGE_LOOP('',(#8118));
#1590=EDGE_LOOP('',(#8119));
#1591=EDGE_LOOP('',(#8120,#8121,#8122,#8123));
#1592=EDGE_LOOP('',(#8124,#8125,#8126,#8127,#8128));
#1593=EDGE_LOOP('',(#8129,#8130,#8131,#8132));
#1594=EDGE_LOOP('',(#8133,#8134,#8135,#8136,#8137));
#1595=EDGE_LOOP('',(#8138,#8139,#8140,#8141,#8142));
#1596=EDGE_LOOP('',(#8143,#8144,#8145,#8146));
#1597=EDGE_LOOP('',(#8147,#8148,#8149,#8150,#8151));
#1598=EDGE_LOOP('',(#8152));
#1599=EDGE_LOOP('',(#8153));
#1600=EDGE_LOOP('',(#8154));
#1601=EDGE_LOOP('',(#8155));
#1602=EDGE_LOOP('',(#8156));
#1603=EDGE_LOOP('',(#8157,#8158,#8159,#8160));
#1604=EDGE_LOOP('',(#8161));
#1605=EDGE_LOOP('',(#8162,#8163,#8164,#8165));
#1606=EDGE_LOOP('',(#8166,#8167,#8168,#8169));
#1607=EDGE_LOOP('',(#8170,#8171,#8172,#8173));
#1608=EDGE_LOOP('',(#8174,#8175,#8176,#8177));
#1609=EDGE_LOOP('',(#8178,#8179,#8180,#8181));
#1610=EDGE_LOOP('',(#8182,#8183,#8184,#8185));
#1611=EDGE_LOOP('',(#8186,#8187,#8188,#8189));
#1612=EDGE_LOOP('',(#8190,#8191,#8192,#8193,#8194));
#1613=EDGE_LOOP('',(#8195,#8196,#8197,#8198));
#1614=EDGE_LOOP('',(#8199,#8200,#8201,#8202,#8203));
#1615=EDGE_LOOP('',(#8204,#8205,#8206,#8207,#8208));
#1616=EDGE_LOOP('',(#8209,#8210,#8211,#8212));
#1617=EDGE_LOOP('',(#8213,#8214,#8215,#8216,#8217));
#1618=EDGE_LOOP('',(#8218));
#1619=EDGE_LOOP('',(#8219));
#1620=EDGE_LOOP('',(#8220));
#1621=EDGE_LOOP('',(#8221));
#1622=EDGE_LOOP('',(#8222));
#1623=EDGE_LOOP('',(#8223));
#1624=EDGE_LOOP('',(#8224));
#1625=EDGE_LOOP('',(#8225));
#1626=EDGE_LOOP('',(#8226,#8227,#8228,#8229,#8230));
#1627=EDGE_LOOP('',(#8231,#8232,#8233,#8234,#8235));
#1628=EDGE_LOOP('',(#8236,#8237,#8238,#8239));
#1629=EDGE_LOOP('',(#8240,#8241,#8242,#8243));
#1630=EDGE_LOOP('',(#8244,#8245,#8246,#8247));
#1631=EDGE_LOOP('',(#8248,#8249,#8250,#8251));
#1632=EDGE_LOOP('',(#8252,#8253,#8254,#8255));
#1633=EDGE_LOOP('',(#8256,#8257,#8258,#8259,#8260,#8261,#8262,#8263,#8264,
#8265,#8266,#8267));
#1634=EDGE_LOOP('',(#8268,#8269,#8270,#8271));
#1635=EDGE_LOOP('',(#8272,#8273,#8274,#8275));
#1636=EDGE_LOOP('',(#8276,#8277,#8278,#8279,#8280));
#1637=EDGE_LOOP('',(#8281,#8282,#8283,#8284,#8285,#8286,#8287,#8288,#8289,
#8290,#8291,#8292));
#1638=EDGE_LOOP('',(#8293,#8294,#8295,#8296,#8297,#8298,#8299,#8300,#8301,
#8302));
#1639=EDGE_LOOP('',(#8303));
#1640=EDGE_LOOP('',(#8304));
#1641=EDGE_LOOP('',(#8305));
#1642=EDGE_LOOP('',(#8306));
#1643=EDGE_LOOP('',(#8307));
#1644=EDGE_LOOP('',(#8308));
#1645=EDGE_LOOP('',(#8309,#8310,#8311,#8312));
#1646=EDGE_LOOP('',(#8313,#8314,#8315,#8316));
#1647=EDGE_LOOP('',(#8317,#8318,#8319,#8320,#8321));
#1648=EDGE_LOOP('',(#8322,#8323,#8324,#8325));
#1649=EDGE_LOOP('',(#8326,#8327,#8328,#8329));
#1650=EDGE_LOOP('',(#8330,#8331,#8332,#8333,#8334));
#1651=EDGE_LOOP('',(#8335,#8336,#8337));
#1652=EDGE_LOOP('',(#8338,#8339,#8340,#8341,#8342,#8343));
#1653=EDGE_LOOP('',(#8344,#8345,#8346));
#1654=EDGE_LOOP('',(#8347,#8348,#8349,#8350,#8351));
#1655=EDGE_LOOP('',(#8352,#8353,#8354,#8355));
#1656=EDGE_LOOP('',(#8356,#8357,#8358,#8359));
#1657=EDGE_LOOP('',(#8360,#8361,#8362,#8363,#8364));
#1658=EDGE_LOOP('',(#8365,#8366,#8367,#8368,#8369,#8370));
#1659=EDGE_LOOP('',(#8371));
#1660=EDGE_LOOP('',(#8372));
#1661=EDGE_LOOP('',(#8373));
#1662=EDGE_LOOP('',(#8374));
#1663=EDGE_LOOP('',(#8375));
#1664=EDGE_LOOP('',(#8376,#8377,#8378,#8379));
#1665=EDGE_LOOP('',(#8380,#8381,#8382,#8383));
#1666=EDGE_LOOP('',(#8384,#8385,#8386,#8387));
#1667=EDGE_LOOP('',(#8388,#8389,#8390,#8391));
#1668=EDGE_LOOP('',(#8392,#8393,#8394,#8395));
#1669=EDGE_LOOP('',(#8396,#8397,#8398,#8399));
#1670=EDGE_LOOP('',(#8400,#8401,#8402,#8403));
#1671=EDGE_LOOP('',(#8404,#8405,#8406,#8407));
#1672=EDGE_LOOP('',(#8408,#8409,#8410,#8411,#8412));
#1673=EDGE_LOOP('',(#8413,#8414));
#1674=EDGE_LOOP('',(#8415,#8416,#8417,#8418));
#1675=EDGE_LOOP('',(#8419,#8420));
#1676=EDGE_LOOP('',(#8421,#8422,#8423,#8424));
#1677=EDGE_LOOP('',(#8425,#8426,#8427,#8428));
#1678=EDGE_LOOP('',(#8429,#8430));
#1679=EDGE_LOOP('',(#8431,#8432,#8433,#8434));
#1680=EDGE_LOOP('',(#8435,#8436));
#1681=EDGE_LOOP('',(#8437,#8438,#8439,#8440));
#1682=EDGE_LOOP('',(#8441));
#1683=EDGE_LOOP('',(#8442,#8443,#8444,#8445));
#1684=EDGE_LOOP('',(#8446,#8447,#8448,#8449));
#1685=EDGE_LOOP('',(#8450));
#1686=EDGE_LOOP('',(#8451,#8452,#8453,#8454));
#1687=EDGE_LOOP('',(#8455,#8456,#8457,#8458));
#1688=EDGE_LOOP('',(#8459));
#1689=EDGE_LOOP('',(#8460,#8461,#8462,#8463));
#1690=EDGE_LOOP('',(#8464,#8465,#8466,#8467));
#1691=EDGE_LOOP('',(#8468,#8469,#8470,#8471));
#1692=EDGE_LOOP('',(#8472,#8473,#8474,#8475));
#1693=EDGE_LOOP('',(#8476,#8477,#8478,#8479));
#1694=EDGE_LOOP('',(#8480,#8481,#8482,#8483));
#1695=EDGE_LOOP('',(#8484,#8485,#8486,#8487));
#1696=EDGE_LOOP('',(#8488,#8489,#8490,#8491));
#1697=EDGE_LOOP('',(#8492,#8493,#8494,#8495));
#1698=EDGE_LOOP('',(#8496,#8497,#8498,#8499));
#1699=EDGE_LOOP('',(#8500,#8501,#8502,#8503));
#1700=EDGE_LOOP('',(#8504,#8505,#8506,#8507));
#1701=EDGE_LOOP('',(#8508,#8509,#8510,#8511));
#1702=EDGE_LOOP('',(#8512,#8513,#8514,#8515));
#1703=EDGE_LOOP('',(#8516,#8517,#8518,#8519,#8520,#8521));
#1704=EDGE_LOOP('',(#8522,#8523,#8524,#8525,#8526,#8527));
#1705=EDGE_LOOP('',(#8528,#8529,#8530,#8531,#8532,#8533));
#1706=EDGE_LOOP('',(#8534,#8535,#8536,#8537,#8538,#8539));
#1707=EDGE_LOOP('',(#8540,#8541,#8542,#8543));
#1708=EDGE_LOOP('',(#8544,#8545,#8546,#8547));
#1709=EDGE_LOOP('',(#8548,#8549,#8550,#8551));
#1710=EDGE_LOOP('',(#8552,#8553,#8554,#8555));
#1711=EDGE_LOOP('',(#8556,#8557,#8558,#8559));
#1712=EDGE_LOOP('',(#8560,#8561,#8562,#8563));
#1713=EDGE_LOOP('',(#8564,#8565,#8566,#8567));
#1714=EDGE_LOOP('',(#8568,#8569,#8570,#8571));
#1715=EDGE_LOOP('',(#8572,#8573,#8574,#8575));
#1716=EDGE_LOOP('',(#8576,#8577,#8578,#8579));
#1717=EDGE_LOOP('',(#8580,#8581,#8582,#8583));
#1718=EDGE_LOOP('',(#8584,#8585,#8586,#8587,#8588,#8589,#8590,#8591,#8592,
#8593,#8594,#8595,#8596,#8597,#8598,#8599,#8600,#8601,#8602,#8603,#8604,
#8605,#8606,#8607,#8608,#8609,#8610,#8611,#8612,#8613,#8614,#8615,#8616,
#8617,#8618,#8619,#8620,#8621,#8622,#8623,#8624,#8625,#8626,#8627,#8628,
#8629,#8630,#8631,#8632,#8633,#8634,#8635,#8636,#8637,#8638,#8639,#8640,
#8641,#8642,#8643,#8644,#8645,#8646,#8647,#8648,#8649,#8650,#8651,#8652,
#8653,#8654,#8655,#8656,#8657,#8658,#8659,#8660,#8661,#8662,#8663,#8664,
#8665,#8666,#8667,#8668,#8669,#8670,#8671,#8672,#8673,#8674,#8675,#8676,
#8677,#8678,#8679,#8680,#8681,#8682,#8683,#8684,#8685,#8686,#8687,#8688,
#8689,#8690,#8691,#8692,#8693,#8694,#8695,#8696,#8697,#8698,#8699));
#1719=EDGE_LOOP('',(#8700,#8701,#8702,#8703,#8704,#8705,#8706,#8707));
#1720=EDGE_LOOP('',(#8708,#8709,#8710,#8711,#8712,#8713,#8714,#8715,#8716,
#8717,#8718,#8719,#8720,#8721,#8722,#8723));
#1721=EDGE_LOOP('',(#8724,#8725,#8726,#8727,#8728,#8729,#8730,#8731));
#1722=EDGE_LOOP('',(#8732,#8733,#8734,#8735,#8736,#8737,#8738,#8739));
#1723=EDGE_LOOP('',(#8740,#8741,#8742,#8743,#8744,#8745,#8746,#8747));
#1724=EDGE_LOOP('',(#8748,#8749,#8750,#8751,#8752,#8753,#8754,#8755,#8756,
#8757,#8758,#8759,#8760,#8761,#8762,#8763,#8764,#8765,#8766,#8767,#8768,
#8769,#8770,#8771,#8772,#8773,#8774,#8775,#8776,#8777,#8778,#8779,#8780,
#8781,#8782,#8783,#8784,#8785,#8786,#8787,#8788,#8789,#8790,#8791,#8792,
#8793,#8794,#8795,#8796,#8797,#8798,#8799,#8800,#8801,#8802,#8803,#8804,
#8805,#8806,#8807,#8808,#8809,#8810,#8811,#8812,#8813,#8814,#8815,#8816,
#8817,#8818,#8819,#8820,#8821,#8822,#8823,#8824,#8825,#8826,#8827,#8828,
#8829,#8830,#8831,#8832,#8833,#8834,#8835,#8836,#8837,#8838,#8839,#8840,
#8841,#8842,#8843,#8844,#8845,#8846,#8847,#8848,#8849,#8850,#8851,#8852,
#8853,#8854,#8855,#8856,#8857,#8858,#8859,#8860,#8861,#8862,#8863));
#1725=EDGE_LOOP('',(#8864,#8865,#8866,#8867,#8868,#8869,#8870,#8871));
#1726=EDGE_LOOP('',(#8872,#8873,#8874,#8875,#8876,#8877,#8878,#8879));
#1727=EDGE_LOOP('',(#8880,#8881,#8882,#8883,#8884,#8885,#8886,#8887));
#1728=EDGE_LOOP('',(#8888,#8889,#8890,#8891,#8892,#8893,#8894,#8895));
#1729=EDGE_LOOP('',(#8896,#8897,#8898,#8899,#8900,#8901,#8902,#8903,#8904,
#8905,#8906,#8907,#8908,#8909,#8910,#8911));
#1730=EDGE_LOOP('',(#8912,#8913,#8914,#8915));
#1731=EDGE_LOOP('',(#8916,#8917,#8918,#8919));
#1732=EDGE_LOOP('',(#8920,#8921,#8922,#8923));
#1733=EDGE_LOOP('',(#8924,#8925,#8926,#8927));
#1734=EDGE_LOOP('',(#8928,#8929,#8930,#8931));
#1735=EDGE_LOOP('',(#8932,#8933,#8934,#8935));
#1736=EDGE_LOOP('',(#8936,#8937,#8938,#8939));
#1737=EDGE_LOOP('',(#8940,#8941,#8942,#8943));
#1738=EDGE_LOOP('',(#8944,#8945,#8946,#8947));
#1739=EDGE_LOOP('',(#8948,#8949,#8950,#8951));
#1740=EDGE_LOOP('',(#8952,#8953,#8954,#8955));
#1741=EDGE_LOOP('',(#8956,#8957,#8958,#8959));
#1742=EDGE_LOOP('',(#8960,#8961,#8962,#8963));
#1743=EDGE_LOOP('',(#8964,#8965,#8966,#8967));
#1744=EDGE_LOOP('',(#8968,#8969,#8970,#8971));
#1745=EDGE_LOOP('',(#8972,#8973,#8974,#8975));
#1746=EDGE_LOOP('',(#8976,#8977,#8978,#8979));
#1747=EDGE_LOOP('',(#8980,#8981,#8982,#8983));
#1748=EDGE_LOOP('',(#8984,#8985,#8986,#8987));
#1749=EDGE_LOOP('',(#8988,#8989,#8990,#8991));
#1750=EDGE_LOOP('',(#8992,#8993,#8994,#8995));
#1751=EDGE_LOOP('',(#8996,#8997,#8998,#8999));
#1752=EDGE_LOOP('',(#9000,#9001,#9002,#9003));
#1753=EDGE_LOOP('',(#9004,#9005,#9006,#9007));
#1754=EDGE_LOOP('',(#9008,#9009,#9010,#9011));
#1755=EDGE_LOOP('',(#9012,#9013,#9014,#9015));
#1756=EDGE_LOOP('',(#9016,#9017,#9018,#9019));
#1757=EDGE_LOOP('',(#9020,#9021,#9022,#9023));
#1758=EDGE_LOOP('',(#9024,#9025,#9026,#9027));
#1759=EDGE_LOOP('',(#9028,#9029,#9030,#9031));
#1760=EDGE_LOOP('',(#9032,#9033,#9034,#9035));
#1761=EDGE_LOOP('',(#9036,#9037,#9038,#9039));
#1762=EDGE_LOOP('',(#9040,#9041,#9042,#9043));
#1763=EDGE_LOOP('',(#9044,#9045,#9046,#9047));
#1764=EDGE_LOOP('',(#9048,#9049,#9050,#9051));
#1765=EDGE_LOOP('',(#9052,#9053,#9054,#9055));
#1766=EDGE_LOOP('',(#9056,#9057,#9058,#9059));
#1767=EDGE_LOOP('',(#9060,#9061,#9062,#9063));
#1768=EDGE_LOOP('',(#9064,#9065,#9066,#9067));
#1769=EDGE_LOOP('',(#9068,#9069,#9070,#9071));
#1770=EDGE_LOOP('',(#9072,#9073,#9074,#9075));
#1771=EDGE_LOOP('',(#9076,#9077,#9078,#9079));
#1772=EDGE_LOOP('',(#9080,#9081,#9082,#9083));
#1773=EDGE_LOOP('',(#9084,#9085,#9086,#9087));
#1774=EDGE_LOOP('',(#9088,#9089,#9090,#9091));
#1775=EDGE_LOOP('',(#9092,#9093,#9094,#9095));
#1776=EDGE_LOOP('',(#9096,#9097,#9098,#9099));
#1777=EDGE_LOOP('',(#9100,#9101,#9102,#9103));
#1778=EDGE_LOOP('',(#9104,#9105,#9106,#9107));
#1779=EDGE_LOOP('',(#9108,#9109,#9110,#9111));
#1780=EDGE_LOOP('',(#9112,#9113,#9114,#9115));
#1781=EDGE_LOOP('',(#9116,#9117,#9118,#9119));
#1782=EDGE_LOOP('',(#9120,#9121,#9122,#9123));
#1783=EDGE_LOOP('',(#9124,#9125,#9126,#9127));
#1784=EDGE_LOOP('',(#9128,#9129,#9130,#9131));
#1785=EDGE_LOOP('',(#9132,#9133,#9134,#9135));
#1786=EDGE_LOOP('',(#9136,#9137,#9138,#9139));
#1787=EDGE_LOOP('',(#9140,#9141,#9142,#9143));
#1788=EDGE_LOOP('',(#9144,#9145,#9146,#9147));
#1789=EDGE_LOOP('',(#9148,#9149,#9150,#9151));
#1790=EDGE_LOOP('',(#9152,#9153,#9154,#9155));
#1791=EDGE_LOOP('',(#9156,#9157,#9158,#9159));
#1792=EDGE_LOOP('',(#9160,#9161,#9162,#9163));
#1793=EDGE_LOOP('',(#9164,#9165,#9166,#9167));
#1794=EDGE_LOOP('',(#9168,#9169,#9170,#9171));
#1795=EDGE_LOOP('',(#9172,#9173,#9174,#9175));
#1796=EDGE_LOOP('',(#9176,#9177,#9178,#9179));
#1797=EDGE_LOOP('',(#9180,#9181,#9182,#9183));
#1798=EDGE_LOOP('',(#9184,#9185,#9186,#9187));
#1799=EDGE_LOOP('',(#9188,#9189,#9190,#9191));
#1800=EDGE_LOOP('',(#9192,#9193,#9194,#9195));
#1801=EDGE_LOOP('',(#9196,#9197,#9198,#9199));
#1802=EDGE_LOOP('',(#9200,#9201,#9202,#9203));
#1803=EDGE_LOOP('',(#9204,#9205,#9206,#9207));
#1804=EDGE_LOOP('',(#9208,#9209,#9210,#9211));
#1805=EDGE_LOOP('',(#9212,#9213,#9214,#9215));
#1806=EDGE_LOOP('',(#9216,#9217,#9218,#9219));
#1807=EDGE_LOOP('',(#9220,#9221,#9222,#9223));
#1808=EDGE_LOOP('',(#9224,#9225,#9226,#9227));
#1809=EDGE_LOOP('',(#9228,#9229,#9230,#9231));
#1810=EDGE_LOOP('',(#9232,#9233,#9234,#9235));
#1811=EDGE_LOOP('',(#9236,#9237,#9238,#9239));
#1812=EDGE_LOOP('',(#9240,#9241,#9242,#9243));
#1813=EDGE_LOOP('',(#9244,#9245,#9246,#9247));
#1814=EDGE_LOOP('',(#9248,#9249,#9250,#9251));
#1815=EDGE_LOOP('',(#9252,#9253,#9254,#9255));
#1816=EDGE_LOOP('',(#9256,#9257,#9258,#9259));
#1817=EDGE_LOOP('',(#9260,#9261,#9262,#9263));
#1818=EDGE_LOOP('',(#9264,#9265,#9266,#9267));
#1819=EDGE_LOOP('',(#9268,#9269,#9270,#9271));
#1820=EDGE_LOOP('',(#9272,#9273,#9274,#9275));
#1821=EDGE_LOOP('',(#9276,#9277,#9278,#9279));
#1822=EDGE_LOOP('',(#9280,#9281,#9282,#9283));
#1823=EDGE_LOOP('',(#9284,#9285,#9286,#9287));
#1824=EDGE_LOOP('',(#9288,#9289,#9290,#9291));
#1825=EDGE_LOOP('',(#9292,#9293,#9294,#9295));
#1826=EDGE_LOOP('',(#9296,#9297,#9298,#9299));
#1827=EDGE_LOOP('',(#9300,#9301,#9302,#9303));
#1828=EDGE_LOOP('',(#9304,#9305,#9306,#9307));
#1829=EDGE_LOOP('',(#9308,#9309,#9310,#9311));
#1830=EDGE_LOOP('',(#9312,#9313,#9314,#9315));
#1831=EDGE_LOOP('',(#9316,#9317,#9318,#9319));
#1832=EDGE_LOOP('',(#9320,#9321,#9322,#9323));
#1833=EDGE_LOOP('',(#9324,#9325,#9326,#9327));
#1834=EDGE_LOOP('',(#9328,#9329,#9330,#9331));
#1835=EDGE_LOOP('',(#9332,#9333,#9334,#9335));
#1836=EDGE_LOOP('',(#9336,#9337,#9338,#9339));
#1837=EDGE_LOOP('',(#9340,#9341,#9342,#9343));
#1838=EDGE_LOOP('',(#9344,#9345,#9346,#9347));
#1839=EDGE_LOOP('',(#9348,#9349,#9350,#9351));
#1840=EDGE_LOOP('',(#9352,#9353,#9354,#9355));
#1841=EDGE_LOOP('',(#9356,#9357,#9358,#9359));
#1842=EDGE_LOOP('',(#9360,#9361,#9362,#9363));
#1843=EDGE_LOOP('',(#9364,#9365,#9366,#9367));
#1844=EDGE_LOOP('',(#9368,#9369,#9370,#9371));
#1845=EDGE_LOOP('',(#9372,#9373,#9374,#9375));
#1846=EDGE_LOOP('',(#9376,#9377,#9378,#9379));
#1847=EDGE_LOOP('',(#9380,#9381,#9382,#9383));
#1848=EDGE_LOOP('',(#9384,#9385,#9386,#9387));
#1849=EDGE_LOOP('',(#9388,#9389,#9390,#9391));
#1850=EDGE_LOOP('',(#9392,#9393,#9394,#9395));
#1851=EDGE_LOOP('',(#9396,#9397,#9398,#9399));
#1852=EDGE_LOOP('',(#9400,#9401,#9402,#9403));
#1853=EDGE_LOOP('',(#9404,#9405,#9406,#9407));
#1854=EDGE_LOOP('',(#9408,#9409,#9410,#9411));
#1855=EDGE_LOOP('',(#9412,#9413,#9414,#9415));
#1856=EDGE_LOOP('',(#9416,#9417,#9418,#9419));
#1857=EDGE_LOOP('',(#9420,#9421,#9422,#9423));
#1858=EDGE_LOOP('',(#9424,#9425,#9426,#9427));
#1859=EDGE_LOOP('',(#9428,#9429,#9430,#9431));
#1860=EDGE_LOOP('',(#9432,#9433,#9434,#9435));
#1861=EDGE_LOOP('',(#9436,#9437,#9438,#9439));
#1862=EDGE_LOOP('',(#9440,#9441,#9442,#9443));
#1863=EDGE_LOOP('',(#9444,#9445,#9446,#9447));
#1864=EDGE_LOOP('',(#9448,#9449,#9450,#9451));
#1865=EDGE_LOOP('',(#9452,#9453,#9454,#9455));
#1866=EDGE_LOOP('',(#9456,#9457,#9458,#9459));
#1867=EDGE_LOOP('',(#9460,#9461,#9462,#9463));
#1868=EDGE_LOOP('',(#9464,#9465,#9466,#9467));
#1869=EDGE_LOOP('',(#9468,#9469,#9470,#9471));
#1870=EDGE_LOOP('',(#9472,#9473,#9474,#9475));
#1871=EDGE_LOOP('',(#9476,#9477,#9478,#9479));
#1872=EDGE_LOOP('',(#9480,#9481,#9482,#9483));
#1873=EDGE_LOOP('',(#9484,#9485,#9486,#9487));
#1874=EDGE_LOOP('',(#9488,#9489,#9490,#9491));
#1875=EDGE_LOOP('',(#9492,#9493,#9494,#9495));
#1876=EDGE_LOOP('',(#9496,#9497,#9498,#9499));
#1877=EDGE_LOOP('',(#9500,#9501,#9502,#9503));
#1878=EDGE_LOOP('',(#9504,#9505,#9506,#9507));
#1879=EDGE_LOOP('',(#9508,#9509,#9510,#9511));
#1880=EDGE_LOOP('',(#9512,#9513,#9514,#9515));
#1881=EDGE_LOOP('',(#9516,#9517,#9518,#9519));
#1882=EDGE_LOOP('',(#9520,#9521,#9522,#9523));
#1883=EDGE_LOOP('',(#9524,#9525,#9526,#9527));
#1884=EDGE_LOOP('',(#9528,#9529,#9530,#9531));
#1885=EDGE_LOOP('',(#9532,#9533,#9534,#9535));
#1886=EDGE_LOOP('',(#9536,#9537,#9538,#9539));
#1887=EDGE_LOOP('',(#9540,#9541,#9542,#9543));
#1888=EDGE_LOOP('',(#9544,#9545,#9546,#9547));
#1889=EDGE_LOOP('',(#9548,#9549,#9550,#9551));
#1890=EDGE_LOOP('',(#9552,#9553,#9554,#9555));
#1891=EDGE_LOOP('',(#9556,#9557,#9558,#9559));
#1892=EDGE_LOOP('',(#9560,#9561,#9562,#9563));
#1893=EDGE_LOOP('',(#9564,#9565,#9566,#9567));
#1894=EDGE_LOOP('',(#9568,#9569,#9570,#9571));
#1895=EDGE_LOOP('',(#9572,#9573,#9574,#9575,#9576));
#1896=EDGE_LOOP('',(#9577,#9578,#9579,#9580,#9581));
#1897=EDGE_LOOP('',(#9582,#9583,#9584,#9585,#9586));
#1898=EDGE_LOOP('',(#9587,#9588,#9589,#9590,#9591,#9592,#9593,#9594));
#1899=EDGE_LOOP('',(#9595,#9596,#9597,#9598,#9599,#9600));
#1900=EDGE_LOOP('',(#9601));
#1901=EDGE_LOOP('',(#9602,#9603,#9604,#9605,#9606,#9607,#9608,#9609));
#1902=EDGE_LOOP('',(#9610,#9611,#9612,#9613,#9614));
#1903=EDGE_LOOP('',(#9615,#9616,#9617,#9618,#9619,#9620,#9621,#9622));
#1904=EDGE_LOOP('',(#9623,#9624,#9625,#9626,#9627,#9628));
#1905=EDGE_LOOP('',(#9629));
#1906=EDGE_LOOP('',(#9630,#9631,#9632,#9633,#9634,#9635,#9636,#9637));
#1907=EDGE_LOOP('',(#9638,#9639,#9640,#9641,#9642,#9643,#9644,#9645,#9646,
#9647,#9648,#9649));
#1908=EDGE_LOOP('',(#9650,#9651,#9652,#9653));
#1909=EDGE_LOOP('',(#9654,#9655,#9656,#9657,#9658,#9659,#9660,#9661,#9662,
#9663,#9664,#9665));
#1910=EDGE_LOOP('',(#9666,#9667,#9668,#9669));
#1911=EDGE_LOOP('',(#9670,#9671,#9672,#9673));
#1912=EDGE_LOOP('',(#9674,#9675,#9676,#9677));
#1913=EDGE_LOOP('',(#9678,#9679,#9680,#9681));
#1914=EDGE_LOOP('',(#9682,#9683,#9684,#9685));
#1915=EDGE_LOOP('',(#9686,#9687,#9688,#9689));
#1916=EDGE_LOOP('',(#9690,#9691,#9692,#9693));
#1917=EDGE_LOOP('',(#9694,#9695,#9696,#9697));
#1918=EDGE_LOOP('',(#9698,#9699,#9700,#9701));
#1919=EDGE_LOOP('',(#9702,#9703,#9704,#9705));
#1920=EDGE_LOOP('',(#9706,#9707,#9708,#9709));
#1921=EDGE_LOOP('',(#9710,#9711,#9712,#9713,#9714,#9715));
#1922=EDGE_LOOP('',(#9716,#9717,#9718,#9719,#9720,#9721));
#1923=EDGE_LOOP('',(#9722,#9723,#9724,#9725));
#1924=EDGE_LOOP('',(#9726));
#1925=EDGE_LOOP('',(#9727,#9728,#9729,#9730,#9731,#9732));
#1926=EDGE_LOOP('',(#9733,#9734,#9735,#9736,#9737,#9738));
#1927=EDGE_LOOP('',(#9739,#9740,#9741,#9742));
#1928=EDGE_LOOP('',(#9743));
#1929=EDGE_LOOP('',(#9744,#9745,#9746,#9747));
#1930=EDGE_LOOP('',(#9748,#9749,#9750,#9751));
#1931=EDGE_LOOP('',(#9752,#9753,#9754,#9755));
#1932=EDGE_LOOP('',(#9756,#9757,#9758,#9759));
#1933=EDGE_LOOP('',(#9760,#9761,#9762,#9763));
#1934=EDGE_LOOP('',(#9764,#9765,#9766,#9767));
#1935=EDGE_LOOP('',(#9768,#9769,#9770,#9771));
#1936=EDGE_LOOP('',(#9772,#9773,#9774,#9775));
#1937=EDGE_LOOP('',(#9776,#9777,#9778,#9779,#9780,#9781));
#1938=EDGE_LOOP('',(#9782,#9783,#9784,#9785,#9786,#9787,#9788,#9789));
#1939=EDGE_LOOP('',(#9790,#9791,#9792,#9793));
#1940=EDGE_LOOP('',(#9794,#9795,#9796,#9797));
#1941=EDGE_LOOP('',(#9798,#9799,#9800,#9801,#9802,#9803,#9804,#9805));
#1942=EDGE_LOOP('',(#9806,#9807,#9808,#9809,#9810,#9811,#9812,#9813));
#1943=EDGE_LOOP('',(#9814,#9815,#9816,#9817));
#1944=EDGE_LOOP('',(#9818,#9819,#9820,#9821,#9822,#9823,#9824,#9825,#9826,
#9827));
#1945=EDGE_LOOP('',(#9828));
#1946=EDGE_LOOP('',(#9829,#9830,#9831,#9832));
#1947=EDGE_LOOP('',(#9833,#9834,#9835,#9836));
#1948=EDGE_LOOP('',(#9837,#9838,#9839,#9840));
#1949=EDGE_LOOP('',(#9841,#9842,#9843,#9844));
#1950=EDGE_LOOP('',(#9845,#9846,#9847,#9848));
#1951=EDGE_LOOP('',(#9849,#9850,#9851,#9852));
#1952=EDGE_LOOP('',(#9853));
#1953=EDGE_LOOP('',(#9854,#9855,#9856,#9857));
#1954=EDGE_LOOP('',(#9858,#9859,#9860,#9861));
#1955=EDGE_LOOP('',(#9862));
#1956=EDGE_LOOP('',(#9863));
#1957=EDGE_LOOP('',(#9864,#9865,#9866,#9867,#9868,#9869,#9870,#9871));
#1958=EDGE_LOOP('',(#9872,#9873,#9874,#9875));
#1959=EDGE_LOOP('',(#9876,#9877,#9878,#9879,#9880,#9881,#9882,#9883));
#1960=EDGE_LOOP('',(#9884,#9885,#9886,#9887));
#1961=EDGE_LOOP('',(#9888,#9889,#9890,#9891));
#1962=EDGE_LOOP('',(#9892,#9893,#9894,#9895));
#1963=EDGE_LOOP('',(#9896,#9897,#9898,#9899));
#1964=EDGE_LOOP('',(#9900,#9901,#9902,#9903));
#1965=EDGE_LOOP('',(#9904,#9905,#9906,#9907));
#1966=EDGE_LOOP('',(#9908,#9909,#9910,#9911));
#1967=EDGE_LOOP('',(#9912,#9913,#9914,#9915));
#1968=EDGE_LOOP('',(#9916,#9917,#9918,#9919));
#1969=EDGE_LOOP('',(#9920,#9921,#9922,#9923));
#1970=EDGE_LOOP('',(#9924,#9925,#9926,#9927));
#1971=EDGE_LOOP('',(#9928,#9929,#9930,#9931));
#1972=EDGE_LOOP('',(#9932,#9933,#9934,#9935));
#1973=EDGE_LOOP('',(#9936,#9937,#9938,#9939));
#1974=EDGE_LOOP('',(#9940,#9941,#9942,#9943,#9944));
#1975=EDGE_LOOP('',(#9945,#9946,#9947,#9948,#9949));
#1976=EDGE_LOOP('',(#9950,#9951,#9952,#9953));
#1977=EDGE_LOOP('',(#9954,#9955,#9956,#9957));
#1978=EDGE_LOOP('',(#9958,#9959,#9960,#9961));
#1979=EDGE_LOOP('',(#9962,#9963,#9964,#9965));
#1980=EDGE_LOOP('',(#9966));
#1981=EDGE_LOOP('',(#9967));
#1982=EDGE_LOOP('',(#9968));
#1983=EDGE_LOOP('',(#9969));
#1984=EDGE_LOOP('',(#9970));
#1985=EDGE_LOOP('',(#9971));
#1986=EDGE_LOOP('',(#9972));
#1987=EDGE_LOOP('',(#9973));
#1988=EDGE_LOOP('',(#9974));
#1989=EDGE_LOOP('',(#9975));
#1990=EDGE_LOOP('',(#9976));
#1991=EDGE_LOOP('',(#9977));
#1992=EDGE_LOOP('',(#9978,#9979));
#1993=EDGE_LOOP('',(#9980,#9981));
#1994=EDGE_LOOP('',(#9982,#9983));
#1995=EDGE_LOOP('',(#9984,#9985));
#1996=EDGE_LOOP('',(#9986,#9987));
#1997=EDGE_LOOP('',(#9988,#9989));
#1998=EDGE_LOOP('',(#9990,#9991));
#1999=EDGE_LOOP('',(#9992,#9993,#9994,#9995));
#2000=EDGE_LOOP('',(#9996,#9997,#9998,#9999));
#2001=EDGE_LOOP('',(#10000,#10001,#10002,#10003));
#2002=EDGE_LOOP('',(#10004,#10005,#10006,#10007));
#2003=EDGE_LOOP('',(#10008,#10009,#10010,#10011));
#2004=EDGE_LOOP('',(#10012,#10013,#10014,#10015));
#2005=EDGE_LOOP('',(#10016,#10017,#10018,#10019));
#2006=EDGE_LOOP('',(#10020,#10021,#10022,#10023));
#2007=EDGE_LOOP('',(#10024,#10025,#10026,#10027,#10028));
#2008=EDGE_LOOP('',(#10029,#10030,#10031,#10032,#10033,#10034));
#2009=EDGE_LOOP('',(#10035,#10036,#10037,#10038,#10039));
#2010=EDGE_LOOP('',(#10040,#10041,#10042,#10043));
#2011=EDGE_LOOP('',(#10044));
#2012=EDGE_LOOP('',(#10045));
#2013=EDGE_LOOP('',(#10046));
#2014=EDGE_LOOP('',(#10047));
#2015=EDGE_LOOP('',(#10048,#10049,#10050,#10051));
#2016=EDGE_LOOP('',(#10052,#10053,#10054,#10055));
#2017=EDGE_LOOP('',(#10056,#10057,#10058,#10059));
#2018=EDGE_LOOP('',(#10060,#10061,#10062,#10063,#10064));
#2019=EDGE_LOOP('',(#10065,#10066,#10067,#10068,#10069));
#2020=EDGE_LOOP('',(#10070,#10071,#10072,#10073,#10074));
#2021=EDGE_LOOP('',(#10075,#10076,#10077,#10078,#10079));
#2022=EDGE_LOOP('',(#10080,#10081,#10082,#10083));
#2023=EDGE_LOOP('',(#10084,#10085,#10086,#10087,#10088));
#2024=EDGE_LOOP('',(#10089,#10090,#10091,#10092,#10093,#10094));
#2025=EDGE_LOOP('',(#10095,#10096,#10097,#10098,#10099,#10100));
#2026=EDGE_LOOP('',(#10101,#10102,#10103,#10104));
#2027=EDGE_LOOP('',(#10105,#10106,#10107,#10108));
#2028=EDGE_LOOP('',(#10109,#10110,#10111,#10112));
#2029=EDGE_LOOP('',(#10113,#10114,#10115,#10116));
#2030=EDGE_LOOP('',(#10117,#10118,#10119,#10120));
#2031=EDGE_LOOP('',(#10121,#10122,#10123,#10124));
#2032=EDGE_LOOP('',(#10125,#10126,#10127,#10128));
#2033=EDGE_LOOP('',(#10129,#10130,#10131,#10132));
#2034=EDGE_LOOP('',(#10133,#10134,#10135,#10136,#10137));
#2035=EDGE_LOOP('',(#10138));
#2036=EDGE_LOOP('',(#10139));
#2037=EDGE_LOOP('',(#10140));
#2038=EDGE_LOOP('',(#10141));
#2039=EDGE_LOOP('',(#10142));
#2040=EDGE_LOOP('',(#10143));
#2041=EDGE_LOOP('',(#10144));
#2042=EDGE_LOOP('',(#10145));
#2043=EDGE_LOOP('',(#10146));
#2044=EDGE_LOOP('',(#10147));
#2045=EDGE_LOOP('',(#10148));
#2046=EDGE_LOOP('',(#10149));
#2047=LINE('',#15611,#3061);
#2048=LINE('',#15617,#3062);
#2049=LINE('',#15623,#3063);
#2050=LINE('',#15629,#3064);
#2051=LINE('',#15635,#3065);
#2052=LINE('',#15641,#3066);
#2053=LINE('',#15647,#3067);
#2054=LINE('',#15653,#3068);
#2055=LINE('',#15659,#3069);
#2056=LINE('',#15664,#3070);
#2057=LINE('',#15666,#3071);
#2058=LINE('',#15668,#3072);
#2059=LINE('',#15670,#3073);
#2060=LINE('',#15672,#3074);
#2061=LINE('',#15674,#3075);
#2062=LINE('',#15676,#3076);
#2063=LINE('',#15678,#3077);
#2064=LINE('',#15680,#3078);
#2065=LINE('',#15681,#3079);
#2066=LINE('',#15684,#3080);
#2067=LINE('',#15686,#3081);
#2068=LINE('',#15689,#3082);
#2069=LINE('',#15692,#3083);
#2070=LINE('',#15694,#3084);
#2071=LINE('',#15697,#3085);
#2072=LINE('',#15701,#3086);
#2073=LINE('',#15703,#3087);
#2074=LINE('',#15705,#3088);
#2075=LINE('',#15707,#3089);
#2076=LINE('',#15710,#3090);
#2077=LINE('',#15712,#3091);
#2078=LINE('',#15713,#3092);
#2079=LINE('',#15716,#3093);
#2080=LINE('',#15718,#3094);
#2081=LINE('',#15720,#3095);
#2082=LINE('',#15722,#3096);
#2083=LINE('',#15724,#3097);
#2084=LINE('',#15725,#3098);
#2085=LINE('',#15728,#3099);
#2086=LINE('',#15730,#3100);
#2087=LINE('',#15732,#3101);
#2088=LINE('',#15734,#3102);
#2089=LINE('',#15736,#3103);
#2090=LINE('',#15737,#3104);
#2091=LINE('',#15740,#3105);
#2092=LINE('',#15742,#3106);
#2093=LINE('',#15743,#3107);
#2094=LINE('',#15746,#3108);
#2095=LINE('',#15750,#3109);
#2096=LINE('',#15751,#3110);
#2097=LINE('',#15753,#3111);
#2098=LINE('',#15754,#3112);
#2099=LINE('',#15757,#3113);
#2100=LINE('',#15759,#3114);
#2101=LINE('',#15761,#3115);
#2102=LINE('',#15762,#3116);
#2103=LINE('',#15764,#3117);
#2104=LINE('',#15765,#3118);
#2105=LINE('',#15768,#3119);
#2106=LINE('',#15769,#3120);
#2107=LINE('',#15777,#3121);
#2108=LINE('',#15778,#3122);
#2109=LINE('',#15781,#3123);
#2110=LINE('',#15782,#3124);
#2111=LINE('',#15785,#3125);
#2112=LINE('',#15787,#3126);
#2113=LINE('',#15788,#3127);
#2114=LINE('',#15795,#3128);
#2115=LINE('',#15797,#3129);
#2116=LINE('',#15798,#3130);
#2117=LINE('',#15801,#3131);
#2118=LINE('',#15802,#3132);
#2119=LINE('',#15805,#3133);
#2120=LINE('',#15806,#3134);
#2121=LINE('',#15809,#3135);
#2122=LINE('',#15810,#3136);
#2123=LINE('',#15813,#3137);
#2124=LINE('',#15814,#3138);
#2125=LINE('',#15816,#3139);
#2126=LINE('',#15820,#3140);
#2127=LINE('',#15822,#3141);
#2128=LINE('',#15823,#3142);
#2129=LINE('',#15826,#3143);
#2130=LINE('',#15827,#3144);
#2131=LINE('',#15830,#3145);
#2132=LINE('',#15831,#3146);
#2133=LINE('',#15834,#3147);
#2134=LINE('',#15835,#3148);
#2135=LINE('',#15838,#3149);
#2136=LINE('',#15839,#3150);
#2137=LINE('',#15841,#3151);
#2138=LINE('',#15844,#3152);
#2139=LINE('',#15846,#3153);
#2140=LINE('',#15849,#3154);
#2141=LINE('',#15850,#3155);
#2142=LINE('',#15858,#3156);
#2143=LINE('',#15864,#3157);
#2144=LINE('',#15870,#3158);
#2145=LINE('',#15876,#3159);
#2146=LINE('',#15882,#3160);
#2147=LINE('',#15888,#3161);
#2148=LINE('',#15894,#3162);
#2149=LINE('',#15900,#3163);
#2150=LINE('',#15906,#3164);
#2151=LINE('',#15911,#3165);
#2152=LINE('',#15913,#3166);
#2153=LINE('',#15915,#3167);
#2154=LINE('',#15917,#3168);
#2155=LINE('',#15919,#3169);
#2156=LINE('',#15921,#3170);
#2157=LINE('',#15923,#3171);
#2158=LINE('',#15925,#3172);
#2159=LINE('',#15927,#3173);
#2160=LINE('',#15928,#3174);
#2161=LINE('',#15931,#3175);
#2162=LINE('',#15933,#3176);
#2163=LINE('',#15936,#3177);
#2164=LINE('',#15939,#3178);
#2165=LINE('',#15941,#3179);
#2166=LINE('',#15944,#3180);
#2167=LINE('',#15948,#3181);
#2168=LINE('',#15950,#3182);
#2169=LINE('',#15951,#3183);
#2170=LINE('',#15953,#3184);
#2171=LINE('',#15957,#3185);
#2172=LINE('',#15959,#3186);
#2173=LINE('',#15960,#3187);
#2174=LINE('',#15963,#3188);
#2175=LINE('',#15965,#3189);
#2176=LINE('',#15967,#3190);
#2177=LINE('',#15969,#3191);
#2178=LINE('',#15971,#3192);
#2179=LINE('',#15972,#3193);
#2180=LINE('',#15975,#3194);
#2181=LINE('',#15977,#3195);
#2182=LINE('',#15979,#3196);
#2183=LINE('',#15981,#3197);
#2184=LINE('',#15983,#3198);
#2185=LINE('',#15984,#3199);
#2186=LINE('',#15987,#3200);
#2187=LINE('',#15989,#3201);
#2188=LINE('',#15990,#3202);
#2189=LINE('',#15994,#3203);
#2190=LINE('',#15997,#3204);
#2191=LINE('',#15998,#3205);
#2192=LINE('',#16000,#3206);
#2193=LINE('',#16001,#3207);
#2194=LINE('',#16004,#3208);
#2195=LINE('',#16006,#3209);
#2196=LINE('',#16007,#3210);
#2197=LINE('',#16009,#3211);
#2198=LINE('',#16011,#3212);
#2199=LINE('',#16012,#3213);
#2200=LINE('',#16015,#3214);
#2201=LINE('',#16016,#3215);
#2202=LINE('',#16024,#3216);
#2203=LINE('',#16025,#3217);
#2204=LINE('',#16028,#3218);
#2205=LINE('',#16029,#3219);
#2206=LINE('',#16032,#3220);
#2207=LINE('',#16034,#3221);
#2208=LINE('',#16035,#3222);
#2209=LINE('',#16042,#3223);
#2210=LINE('',#16044,#3224);
#2211=LINE('',#16045,#3225);
#2212=LINE('',#16048,#3226);
#2213=LINE('',#16049,#3227);
#2214=LINE('',#16052,#3228);
#2215=LINE('',#16053,#3229);
#2216=LINE('',#16056,#3230);
#2217=LINE('',#16057,#3231);
#2218=LINE('',#16060,#3232);
#2219=LINE('',#16061,#3233);
#2220=LINE('',#16063,#3234);
#2221=LINE('',#16067,#3235);
#2222=LINE('',#16069,#3236);
#2223=LINE('',#16070,#3237);
#2224=LINE('',#16073,#3238);
#2225=LINE('',#16074,#3239);
#2226=LINE('',#16077,#3240);
#2227=LINE('',#16078,#3241);
#2228=LINE('',#16081,#3242);
#2229=LINE('',#16082,#3243);
#2230=LINE('',#16085,#3244);
#2231=LINE('',#16086,#3245);
#2232=LINE('',#16088,#3246);
#2233=LINE('',#16091,#3247);
#2234=LINE('',#16093,#3248);
#2235=LINE('',#16096,#3249);
#2236=LINE('',#16097,#3250);
#2237=LINE('',#16105,#3251);
#2238=LINE('',#16115,#3252);
#2239=LINE('',#16121,#3253);
#2240=LINE('',#16127,#3254);
#2241=LINE('',#16133,#3255);
#2242=LINE('',#16139,#3256);
#2243=LINE('',#16145,#3257);
#2244=LINE('',#16150,#3258);
#2245=LINE('',#16152,#3259);
#2246=LINE('',#16154,#3260);
#2247=LINE('',#16157,#3261);
#2248=LINE('',#16161,#3262);
#2249=LINE('',#16163,#3263);
#2250=LINE('',#16167,#3264);
#2251=LINE('',#16168,#3265);
#2252=LINE('',#16171,#3266);
#2253=LINE('',#16173,#3267);
#2254=LINE('',#16174,#3268);
#2255=LINE('',#16176,#3269);
#2256=LINE('',#16178,#3270);
#2257=LINE('',#16179,#3271);
#2258=LINE('',#16182,#3272);
#2259=LINE('',#16184,#3273);
#2260=LINE('',#16186,#3274);
#2261=LINE('',#16187,#3275);
#2262=LINE('',#16193,#3276);
#2263=LINE('',#16195,#3277);
#2264=LINE('',#16197,#3278);
#2265=LINE('',#16198,#3279);
#2266=LINE('',#16201,#3280);
#2267=LINE('',#16203,#3281);
#2268=LINE('',#16205,#3282);
#2269=LINE('',#16209,#3283);
#2270=LINE('',#16213,#3284);
#2271=LINE('',#16215,#3285);
#2272=LINE('',#16216,#3286);
#2273=LINE('',#16218,#3287);
#2274=LINE('',#16220,#3288);
#2275=LINE('',#16221,#3289);
#2276=LINE('',#16224,#3290);
#2277=LINE('',#16225,#3291);
#2278=LINE('',#16228,#3292);
#2279=LINE('',#16232,#3293);
#2280=LINE('',#16233,#3294);
#2281=LINE('',#16234,#3295);
#2282=LINE('',#16245,#3296);
#2283=LINE('',#16246,#3297);
#2284=LINE('',#16247,#3298);
#2285=LINE('',#16252,#3299);
#2286=LINE('',#16256,#3300);
#2287=LINE('',#16257,#3301);
#2288=LINE('',#16259,#3302);
#2289=LINE('',#16260,#3303);
#2290=LINE('',#16262,#3304);
#2291=LINE('',#16263,#3305);
#2292=LINE('',#16268,#3306);
#2293=LINE('',#16269,#3307);
#2294=LINE('',#16277,#3308);
#2295=LINE('',#16287,#3309);
#2296=LINE('',#16293,#3310);
#2297=LINE('',#16299,#3311);
#2298=LINE('',#16305,#3312);
#2299=LINE('',#16311,#3313);
#2300=LINE('',#16317,#3314);
#2301=LINE('',#16322,#3315);
#2302=LINE('',#16324,#3316);
#2303=LINE('',#16328,#3317);
#2304=LINE('',#16329,#3318);
#2305=LINE('',#16333,#3319);
#2306=LINE('',#16335,#3320);
#2307=LINE('',#16337,#3321);
#2308=LINE('',#16340,#3322);
#2309=LINE('',#16343,#3323);
#2310=LINE('',#16345,#3324);
#2311=LINE('',#16347,#3325);
#2312=LINE('',#16348,#3326);
#2313=LINE('',#16350,#3327);
#2314=LINE('',#16351,#3328);
#2315=LINE('',#16354,#3329);
#2316=LINE('',#16356,#3330);
#2317=LINE('',#16358,#3331);
#2318=LINE('',#16359,#3332);
#2319=LINE('',#16364,#3333);
#2320=LINE('',#16368,#3334);
#2321=LINE('',#16369,#3335);
#2322=LINE('',#16370,#3336);
#2323=LINE('',#16373,#3337);
#2324=LINE('',#16375,#3338);
#2325=LINE('',#16377,#3339);
#2326=LINE('',#16378,#3340);
#2327=LINE('',#16380,#3341);
#2328=LINE('',#16382,#3342);
#2329=LINE('',#16384,#3343);
#2330=LINE('',#16388,#3344);
#2331=LINE('',#16392,#3345);
#2332=LINE('',#16393,#3346);
#2333=LINE('',#16396,#3347);
#2334=LINE('',#16397,#3348);
#2335=LINE('',#16400,#3349);
#2336=LINE('',#16401,#3350);
#2337=LINE('',#16403,#3351);
#2338=LINE('',#16404,#3352);
#2339=LINE('',#16417,#3353);
#2340=LINE('',#16418,#3354);
#2341=LINE('',#16419,#3355);
#2342=LINE('',#16422,#3356);
#2343=LINE('',#16424,#3357);
#2344=LINE('',#16428,#3358);
#2345=LINE('',#16431,#3359);
#2346=LINE('',#16432,#3360);
#2347=LINE('',#16434,#3361);
#2348=LINE('',#16435,#3362);
#2349=LINE('',#16440,#3363);
#2350=LINE('',#16441,#3364);
#2351=LINE('',#16449,#3365);
#2352=LINE('',#16455,#3366);
#2353=LINE('',#16461,#3367);
#2354=LINE('',#16467,#3368);
#2355=LINE('',#16473,#3369);
#2356=LINE('',#16479,#3370);
#2357=LINE('',#16485,#3371);
#2358=LINE('',#16491,#3372);
#2359=LINE('',#16497,#3373);
#2360=LINE('',#16503,#3374);
#2361=LINE('',#16508,#3375);
#2362=LINE('',#16510,#3376);
#2363=LINE('',#16512,#3377);
#2364=LINE('',#16513,#3378);
#2365=LINE('',#16517,#3379);
#2366=LINE('',#16519,#3380);
#2367=LINE('',#16521,#3381);
#2368=LINE('',#16522,#3382);
#2369=LINE('',#16526,#3383);
#2370=LINE('',#16528,#3384);
#2371=LINE('',#16530,#3385);
#2372=LINE('',#16531,#3386);
#2373=LINE('',#16541,#3387);
#2374=LINE('',#16543,#3388);
#2375=LINE('',#16545,#3389);
#2376=LINE('',#16546,#3390);
#2377=LINE('',#16551,#3391);
#2378=LINE('',#16555,#3392);
#2379=LINE('',#16557,#3393);
#2380=LINE('',#16558,#3394);
#2381=LINE('',#16563,#3395);
#2382=LINE('',#16567,#3396);
#2383=LINE('',#16569,#3397);
#2384=LINE('',#16570,#3398);
#2385=LINE('',#16575,#3399);
#2386=LINE('',#16579,#3400);
#2387=LINE('',#16581,#3401);
#2388=LINE('',#16582,#3402);
#2389=LINE('',#16589,#3403);
#2390=LINE('',#16591,#3404);
#2391=LINE('',#16593,#3405);
#2392=LINE('',#16594,#3406);
#2393=LINE('',#16598,#3407);
#2394=LINE('',#16600,#3408);
#2395=LINE('',#16602,#3409);
#2396=LINE('',#16603,#3410);
#2397=LINE('',#16607,#3411);
#2398=LINE('',#16609,#3412);
#2399=LINE('',#16611,#3413);
#2400=LINE('',#16612,#3414);
#2401=LINE('',#16616,#3415);
#2402=LINE('',#16618,#3416);
#2403=LINE('',#16620,#3417);
#2404=LINE('',#16621,#3418);
#2405=LINE('',#16625,#3419);
#2406=LINE('',#16627,#3420);
#2407=LINE('',#16629,#3421);
#2408=LINE('',#16630,#3422);
#2409=LINE('',#16685,#3423);
#2410=LINE('',#16690,#3424);
#2411=LINE('',#16693,#3425);
#2412=LINE('',#16701,#3426);
#2413=LINE('',#16704,#3427);
#2414=LINE('',#16710,#3428);
#2415=LINE('',#16713,#3429);
#2416=LINE('',#16715,#3430);
#2417=LINE('',#16716,#3431);
#2418=LINE('',#16718,#3432);
#2419=LINE('',#16720,#3433);
#2420=LINE('',#16727,#3434);
#2421=LINE('',#16758,#3435);
#2422=LINE('',#16763,#3436);
#2423=LINE('',#16766,#3437);
#2424=LINE('',#16783,#3438);
#2425=LINE('',#16788,#3439);
#2426=LINE('',#16794,#3440);
#2427=LINE('',#16800,#3441);
#2428=LINE('',#16806,#3442);
#2429=LINE('',#16812,#3443);
#2430=LINE('',#16818,#3444);
#2431=LINE('',#16822,#3445);
#2432=LINE('',#16826,#3446);
#2433=LINE('',#16830,#3447);
#2434=LINE('',#16834,#3448);
#2435=LINE('',#16876,#3449);
#2436=LINE('',#16879,#3450);
#2437=LINE('',#16885,#3451);
#2438=LINE('',#16890,#3452);
#2439=LINE('',#16895,#3453);
#2440=LINE('',#16899,#3454);
#2441=LINE('',#16903,#3455);
#2442=LINE('',#16907,#3456);
#2443=LINE('',#16911,#3457);
#2444=LINE('',#16915,#3458);
#2445=LINE('',#16917,#3459);
#2446=LINE('',#16921,#3460);
#2447=LINE('',#16925,#3461);
#2448=LINE('',#16927,#3462);
#2449=LINE('',#16929,#3463);
#2450=LINE('',#16930,#3464);
#2451=LINE('',#16934,#3465);
#2452=LINE('',#16935,#3466);
#2453=LINE('',#16936,#3467);
#2454=LINE('',#16939,#3468);
#2455=LINE('',#16941,#3469);
#2456=LINE('',#16943,#3470);
#2457=LINE('',#16944,#3471);
#2458=LINE('',#16946,#3472);
#2459=LINE('',#16947,#3473);
#2460=LINE('',#16951,#3474);
#2461=LINE('',#16953,#3475);
#2462=LINE('',#16956,#3476);
#2463=LINE('',#16962,#3477);
#2464=LINE('',#16964,#3478);
#2465=LINE('',#16967,#3479);
#2466=LINE('',#16969,#3480);
#2467=LINE('',#16970,#3481);
#2468=LINE('',#16971,#3482);
#2469=LINE('',#16973,#3483);
#2470=LINE('',#16976,#3484);
#2471=LINE('',#16977,#3485);
#2472=LINE('',#16983,#3486);
#2473=LINE('',#16985,#3487);
#2474=LINE('',#16989,#3488);
#2475=LINE('',#16990,#3489);
#2476=LINE('',#16992,#3490);
#2477=LINE('',#16994,#3491);
#2478=LINE('',#16999,#3492);
#2479=LINE('',#17000,#3493);
#2480=LINE('',#17033,#3494);
#2481=LINE('',#17034,#3495);
#2482=LINE('',#17036,#3496);
#2483=LINE('',#17039,#3497);
#2484=LINE('',#17042,#3498);
#2485=LINE('',#17045,#3499);
#2486=LINE('',#17049,#3500);
#2487=LINE('',#17051,#3501);
#2488=LINE('',#17052,#3502);
#2489=LINE('',#17055,#3503);
#2490=LINE('',#17056,#3504);
#2491=LINE('',#17059,#3505);
#2492=LINE('',#17060,#3506);
#2493=LINE('',#17062,#3507);
#2494=LINE('',#17071,#3508);
#2495=LINE('',#17074,#3509);
#2496=LINE('',#17080,#3510);
#2497=LINE('',#17083,#3511);
#2498=LINE('',#17086,#3512);
#2499=LINE('',#17089,#3513);
#2500=LINE('',#17091,#3514);
#2501=LINE('',#17093,#3515);
#2502=LINE('',#17097,#3516);
#2503=LINE('',#17100,#3517);
#2504=LINE('',#17102,#3518);
#2505=LINE('',#17105,#3519);
#2506=LINE('',#17107,#3520);
#2507=LINE('',#17109,#3521);
#2508=LINE('',#17112,#3522);
#2509=LINE('',#17114,#3523);
#2510=LINE('',#17122,#3524);
#2511=LINE('',#17125,#3525);
#2512=LINE('',#17131,#3526);
#2513=LINE('',#17134,#3527);
#2514=LINE('',#17137,#3528);
#2515=LINE('',#17139,#3529);
#2516=LINE('',#17141,#3530);
#2517=LINE('',#17144,#3531);
#2518=LINE('',#17146,#3532);
#2519=LINE('',#17148,#3533);
#2520=LINE('',#17152,#3534);
#2521=LINE('',#17153,#3535);
#2522=LINE('',#17156,#3536);
#2523=LINE('',#17160,#3537);
#2524=LINE('',#17162,#3538);
#2525=LINE('',#17163,#3539);
#2526=LINE('',#17165,#3540);
#2527=LINE('',#17167,#3541);
#2528=LINE('',#17169,#3542);
#2529=LINE('',#17172,#3543);
#2530=LINE('',#17174,#3544);
#2531=LINE('',#17176,#3545);
#2532=LINE('',#17178,#3546);
#2533=LINE('',#17180,#3547);
#2534=LINE('',#17183,#3548);
#2535=LINE('',#17185,#3549);
#2536=LINE('',#17187,#3550);
#2537=LINE('',#17189,#3551);
#2538=LINE('',#17197,#3552);
#2539=LINE('',#17200,#3553);
#2540=LINE('',#17204,#3554);
#2541=LINE('',#17206,#3555);
#2542=LINE('',#17208,#3556);
#2543=LINE('',#17210,#3557);
#2544=LINE('',#17212,#3558);
#2545=LINE('',#17216,#3559);
#2546=LINE('',#17220,#3560);
#2547=LINE('',#17224,#3561);
#2548=LINE('',#17228,#3562);
#2549=LINE('',#17232,#3563);
#2550=LINE('',#17236,#3564);
#2551=LINE('',#17240,#3565);
#2552=LINE('',#17244,#3566);
#2553=LINE('',#17248,#3567);
#2554=LINE('',#17252,#3568);
#2555=LINE('',#17256,#3569);
#2556=LINE('',#17258,#3570);
#2557=LINE('',#17260,#3571);
#2558=LINE('',#17262,#3572);
#2559=LINE('',#17264,#3573);
#2560=LINE('',#17266,#3574);
#2561=LINE('',#17268,#3575);
#2562=LINE('',#17270,#3576);
#2563=LINE('',#17274,#3577);
#2564=LINE('',#17278,#3578);
#2565=LINE('',#17282,#3579);
#2566=LINE('',#17286,#3580);
#2567=LINE('',#17290,#3581);
#2568=LINE('',#17294,#3582);
#2569=LINE('',#17298,#3583);
#2570=LINE('',#17302,#3584);
#2571=LINE('',#17306,#3585);
#2572=LINE('',#17310,#3586);
#2573=LINE('',#17314,#3587);
#2574=LINE('',#17316,#3588);
#2575=LINE('',#17318,#3589);
#2576=LINE('',#17320,#3590);
#2577=LINE('',#17322,#3591);
#2578=LINE('',#17324,#3592);
#2579=LINE('',#17326,#3593);
#2580=LINE('',#17328,#3594);
#2581=LINE('',#17332,#3595);
#2582=LINE('',#17336,#3596);
#2583=LINE('',#17340,#3597);
#2584=LINE('',#17344,#3598);
#2585=LINE('',#17348,#3599);
#2586=LINE('',#17352,#3600);
#2587=LINE('',#17356,#3601);
#2588=LINE('',#17360,#3602);
#2589=LINE('',#17364,#3603);
#2590=LINE('',#17368,#3604);
#2591=LINE('',#17372,#3605);
#2592=LINE('',#17374,#3606);
#2593=LINE('',#17376,#3607);
#2594=LINE('',#17378,#3608);
#2595=LINE('',#17380,#3609);
#2596=LINE('',#17382,#3610);
#2597=LINE('',#17384,#3611);
#2598=LINE('',#17386,#3612);
#2599=LINE('',#17390,#3613);
#2600=LINE('',#17394,#3614);
#2601=LINE('',#17398,#3615);
#2602=LINE('',#17402,#3616);
#2603=LINE('',#17406,#3617);
#2604=LINE('',#17410,#3618);
#2605=LINE('',#17414,#3619);
#2606=LINE('',#17418,#3620);
#2607=LINE('',#17422,#3621);
#2608=LINE('',#17426,#3622);
#2609=LINE('',#17430,#3623);
#2610=LINE('',#17432,#3624);
#2611=LINE('',#17433,#3625);
#2612=LINE('',#17436,#3626);
#2613=LINE('',#17440,#3627);
#2614=LINE('',#17444,#3628);
#2615=LINE('',#17448,#3629);
#2616=LINE('',#17452,#3630);
#2617=LINE('',#17456,#3631);
#2618=LINE('',#17460,#3632);
#2619=LINE('',#17464,#3633);
#2620=LINE('',#17468,#3634);
#2621=LINE('',#17472,#3635);
#2622=LINE('',#17475,#3636);
#2623=LINE('',#17477,#3637);
#2624=LINE('',#17481,#3638);
#2625=LINE('',#17485,#3639);
#2626=LINE('',#17489,#3640);
#2627=LINE('',#17493,#3641);
#2628=LINE('',#17497,#3642);
#2629=LINE('',#17501,#3643);
#2630=LINE('',#17505,#3644);
#2631=LINE('',#17509,#3645);
#2632=LINE('',#17513,#3646);
#2633=LINE('',#17517,#3647);
#2634=LINE('',#17521,#3648);
#2635=LINE('',#17525,#3649);
#2636=LINE('',#17530,#3650);
#2637=LINE('',#17532,#3651);
#2638=LINE('',#17534,#3652);
#2639=LINE('',#17536,#3653);
#2640=LINE('',#17540,#3654);
#2641=LINE('',#17544,#3655);
#2642=LINE('',#17548,#3656);
#2643=LINE('',#17552,#3657);
#2644=LINE('',#17556,#3658);
#2645=LINE('',#17560,#3659);
#2646=LINE('',#17564,#3660);
#2647=LINE('',#17568,#3661);
#2648=LINE('',#17572,#3662);
#2649=LINE('',#17576,#3663);
#2650=LINE('',#17580,#3664);
#2651=LINE('',#17582,#3665);
#2652=LINE('',#17584,#3666);
#2653=LINE('',#17586,#3667);
#2654=LINE('',#17588,#3668);
#2655=LINE('',#17590,#3669);
#2656=LINE('',#17592,#3670);
#2657=LINE('',#17594,#3671);
#2658=LINE('',#17598,#3672);
#2659=LINE('',#17602,#3673);
#2660=LINE('',#17606,#3674);
#2661=LINE('',#17610,#3675);
#2662=LINE('',#17614,#3676);
#2663=LINE('',#17618,#3677);
#2664=LINE('',#17622,#3678);
#2665=LINE('',#17626,#3679);
#2666=LINE('',#17630,#3680);
#2667=LINE('',#17634,#3681);
#2668=LINE('',#17638,#3682);
#2669=LINE('',#17640,#3683);
#2670=LINE('',#17642,#3684);
#2671=LINE('',#17644,#3685);
#2672=LINE('',#17646,#3686);
#2673=LINE('',#17648,#3687);
#2674=LINE('',#17650,#3688);
#2675=LINE('',#17652,#3689);
#2676=LINE('',#17656,#3690);
#2677=LINE('',#17660,#3691);
#2678=LINE('',#17664,#3692);
#2679=LINE('',#17668,#3693);
#2680=LINE('',#17672,#3694);
#2681=LINE('',#17676,#3695);
#2682=LINE('',#17680,#3696);
#2683=LINE('',#17684,#3697);
#2684=LINE('',#17688,#3698);
#2685=LINE('',#17692,#3699);
#2686=LINE('',#17696,#3700);
#2687=LINE('',#17698,#3701);
#2688=LINE('',#17700,#3702);
#2689=LINE('',#17702,#3703);
#2690=LINE('',#17704,#3704);
#2691=LINE('',#17706,#3705);
#2692=LINE('',#17708,#3706);
#2693=LINE('',#17710,#3707);
#2694=LINE('',#17714,#3708);
#2695=LINE('',#17718,#3709);
#2696=LINE('',#17722,#3710);
#2697=LINE('',#17726,#3711);
#2698=LINE('',#17730,#3712);
#2699=LINE('',#17734,#3713);
#2700=LINE('',#17738,#3714);
#2701=LINE('',#17742,#3715);
#2702=LINE('',#17746,#3716);
#2703=LINE('',#17750,#3717);
#2704=LINE('',#17754,#3718);
#2705=LINE('',#17756,#3719);
#2706=LINE('',#17758,#3720);
#2707=LINE('',#17759,#3721);
#2708=LINE('',#17764,#3722);
#2709=LINE('',#17768,#3723);
#2710=LINE('',#17772,#3724);
#2711=LINE('',#17775,#3725);
#2712=LINE('',#17780,#3726);
#2713=LINE('',#17784,#3727);
#2714=LINE('',#17788,#3728);
#2715=LINE('',#17791,#3729);
#2716=LINE('',#17796,#3730);
#2717=LINE('',#17800,#3731);
#2718=LINE('',#17804,#3732);
#2719=LINE('',#17807,#3733);
#2720=LINE('',#17812,#3734);
#2721=LINE('',#17816,#3735);
#2722=LINE('',#17820,#3736);
#2723=LINE('',#17823,#3737);
#2724=LINE('',#17828,#3738);
#2725=LINE('',#17831,#3739);
#2726=LINE('',#17833,#3740);
#2727=LINE('',#17837,#3741);
#2728=LINE('',#17841,#3742);
#2729=LINE('',#17845,#3743);
#2730=LINE('',#17849,#3744);
#2731=LINE('',#17852,#3745);
#2732=LINE('',#17854,#3746);
#2733=LINE('',#17855,#3747);
#2734=LINE('',#17857,#3748);
#2735=LINE('',#17859,#3749);
#2736=LINE('',#17861,#3750);
#2737=LINE('',#17863,#3751);
#2738=LINE('',#17865,#3752);
#2739=LINE('',#17867,#3753);
#2740=LINE('',#17869,#3754);
#2741=LINE('',#17871,#3755);
#2742=LINE('',#17873,#3756);
#2743=LINE('',#17875,#3757);
#2744=LINE('',#17877,#3758);
#2745=LINE('',#17879,#3759);
#2746=LINE('',#17881,#3760);
#2747=LINE('',#17883,#3761);
#2748=LINE('',#17885,#3762);
#2749=LINE('',#17887,#3763);
#2750=LINE('',#17889,#3764);
#2751=LINE('',#17891,#3765);
#2752=LINE('',#17893,#3766);
#2753=LINE('',#17895,#3767);
#2754=LINE('',#17897,#3768);
#2755=LINE('',#17899,#3769);
#2756=LINE('',#17901,#3770);
#2757=LINE('',#17903,#3771);
#2758=LINE('',#17905,#3772);
#2759=LINE('',#17907,#3773);
#2760=LINE('',#17909,#3774);
#2761=LINE('',#17911,#3775);
#2762=LINE('',#17913,#3776);
#2763=LINE('',#17915,#3777);
#2764=LINE('',#17917,#3778);
#2765=LINE('',#17919,#3779);
#2766=LINE('',#17921,#3780);
#2767=LINE('',#17923,#3781);
#2768=LINE('',#17925,#3782);
#2769=LINE('',#17927,#3783);
#2770=LINE('',#17929,#3784);
#2771=LINE('',#17931,#3785);
#2772=LINE('',#17933,#3786);
#2773=LINE('',#17935,#3787);
#2774=LINE('',#17937,#3788);
#2775=LINE('',#17939,#3789);
#2776=LINE('',#17941,#3790);
#2777=LINE('',#17943,#3791);
#2778=LINE('',#17945,#3792);
#2779=LINE('',#17947,#3793);
#2780=LINE('',#17949,#3794);
#2781=LINE('',#17951,#3795);
#2782=LINE('',#17953,#3796);
#2783=LINE('',#17955,#3797);
#2784=LINE('',#17957,#3798);
#2785=LINE('',#17959,#3799);
#2786=LINE('',#17961,#3800);
#2787=LINE('',#17963,#3801);
#2788=LINE('',#17965,#3802);
#2789=LINE('',#17967,#3803);
#2790=LINE('',#17969,#3804);
#2791=LINE('',#17971,#3805);
#2792=LINE('',#17973,#3806);
#2793=LINE('',#17975,#3807);
#2794=LINE('',#17977,#3808);
#2795=LINE('',#17979,#3809);
#2796=LINE('',#17981,#3810);
#2797=LINE('',#17983,#3811);
#2798=LINE('',#17985,#3812);
#2799=LINE('',#17987,#3813);
#2800=LINE('',#17989,#3814);
#2801=LINE('',#17991,#3815);
#2802=LINE('',#17993,#3816);
#2803=LINE('',#17995,#3817);
#2804=LINE('',#17997,#3818);
#2805=LINE('',#17999,#3819);
#2806=LINE('',#18001,#3820);
#2807=LINE('',#18003,#3821);
#2808=LINE('',#18005,#3822);
#2809=LINE('',#18007,#3823);
#2810=LINE('',#18009,#3824);
#2811=LINE('',#18011,#3825);
#2812=LINE('',#18013,#3826);
#2813=LINE('',#18015,#3827);
#2814=LINE('',#18017,#3828);
#2815=LINE('',#18019,#3829);
#2816=LINE('',#18021,#3830);
#2817=LINE('',#18023,#3831);
#2818=LINE('',#18025,#3832);
#2819=LINE('',#18027,#3833);
#2820=LINE('',#18029,#3834);
#2821=LINE('',#18031,#3835);
#2822=LINE('',#18033,#3836);
#2823=LINE('',#18035,#3837);
#2824=LINE('',#18037,#3838);
#2825=LINE('',#18039,#3839);
#2826=LINE('',#18041,#3840);
#2827=LINE('',#18043,#3841);
#2828=LINE('',#18045,#3842);
#2829=LINE('',#18047,#3843);
#2830=LINE('',#18049,#3844);
#2831=LINE('',#18051,#3845);
#2832=LINE('',#18053,#3846);
#2833=LINE('',#18055,#3847);
#2834=LINE('',#18057,#3848);
#2835=LINE('',#18059,#3849);
#2836=LINE('',#18061,#3850);
#2837=LINE('',#18063,#3851);
#2838=LINE('',#18065,#3852);
#2839=LINE('',#18067,#3853);
#2840=LINE('',#18069,#3854);
#2841=LINE('',#18071,#3855);
#2842=LINE('',#18073,#3856);
#2843=LINE('',#18075,#3857);
#2844=LINE('',#18077,#3858);
#2845=LINE('',#18079,#3859);
#2846=LINE('',#18081,#3860);
#2847=LINE('',#18083,#3861);
#2848=LINE('',#18086,#3862);
#2849=LINE('',#18087,#3863);
#2850=LINE('',#18089,#3864);
#2851=LINE('',#18091,#3865);
#2852=LINE('',#18093,#3866);
#2853=LINE('',#18095,#3867);
#2854=LINE('',#18097,#3868);
#2855=LINE('',#18099,#3869);
#2856=LINE('',#18102,#3870);
#2857=LINE('',#18103,#3871);
#2858=LINE('',#18105,#3872);
#2859=LINE('',#18107,#3873);
#2860=LINE('',#18110,#3874);
#2861=LINE('',#18112,#3875);
#2862=LINE('',#18114,#3876);
#2863=LINE('',#18116,#3877);
#2864=LINE('',#18118,#3878);
#2865=LINE('',#18120,#3879);
#2866=LINE('',#18122,#3880);
#2867=LINE('',#18124,#3881);
#2868=LINE('',#18126,#3882);
#2869=LINE('',#18128,#3883);
#2870=LINE('',#18131,#3884);
#2871=LINE('',#18132,#3885);
#2872=LINE('',#18134,#3886);
#2873=LINE('',#18136,#3887);
#2874=LINE('',#18138,#3888);
#2875=LINE('',#18140,#3889);
#2876=LINE('',#18142,#3890);
#2877=LINE('',#18144,#3891);
#2878=LINE('',#18147,#3892);
#2879=LINE('',#18148,#3893);
#2880=LINE('',#18150,#3894);
#2881=LINE('',#18152,#3895);
#2882=LINE('',#18154,#3896);
#2883=LINE('',#18156,#3897);
#2884=LINE('',#18158,#3898);
#2885=LINE('',#18160,#3899);
#2886=LINE('',#18163,#3900);
#2887=LINE('',#18164,#3901);
#2888=LINE('',#18166,#3902);
#2889=LINE('',#18168,#3903);
#2890=LINE('',#18170,#3904);
#2891=LINE('',#18172,#3905);
#2892=LINE('',#18174,#3906);
#2893=LINE('',#18176,#3907);
#2894=LINE('',#18183,#3908);
#2895=LINE('',#18189,#3909);
#2896=LINE('',#18194,#3910);
#2897=LINE('',#18196,#3911);
#2898=LINE('',#18198,#3912);
#2899=LINE('',#18200,#3913);
#2900=LINE('',#18205,#3914);
#2901=LINE('',#18207,#3915);
#2902=LINE('',#18209,#3916);
#2903=LINE('',#18211,#3917);
#2904=LINE('',#18216,#3918);
#2905=LINE('',#18218,#3919);
#2906=LINE('',#18220,#3920);
#2907=LINE('',#18223,#3921);
#2908=LINE('',#18226,#3922);
#2909=LINE('',#18228,#3923);
#2910=LINE('',#18229,#3924);
#2911=LINE('',#18231,#3925);
#2912=LINE('',#18233,#3926);
#2913=LINE('',#18234,#3927);
#2914=LINE('',#18239,#3928);
#2915=LINE('',#18241,#3929);
#2916=LINE('',#18243,#3930);
#2917=LINE('',#18248,#3931);
#2918=LINE('',#18250,#3932);
#2919=LINE('',#18252,#3933);
#2920=LINE('',#18254,#3934);
#2921=LINE('',#18256,#3935);
#2922=LINE('',#18258,#3936);
#2923=LINE('',#18260,#3937);
#2924=LINE('',#18261,#3938);
#2925=LINE('',#18265,#3939);
#2926=LINE('',#18267,#3940);
#2927=LINE('',#18269,#3941);
#2928=LINE('',#18272,#3942);
#2929=LINE('',#18276,#3943);
#2930=LINE('',#18277,#3944);
#2931=LINE('',#18279,#3945);
#2932=LINE('',#18281,#3946);
#2933=LINE('',#18282,#3947);
#2934=LINE('',#18283,#3948);
#2935=LINE('',#18287,#3949);
#2936=LINE('',#18292,#3950);
#2937=LINE('',#18293,#3951);
#2938=LINE('',#18297,#3952);
#2939=LINE('',#18299,#3953);
#2940=LINE('',#18301,#3954);
#2941=LINE('',#18303,#3955);
#2942=LINE('',#18305,#3956);
#2943=LINE('',#18307,#3957);
#2944=LINE('',#18309,#3958);
#2945=LINE('',#18310,#3959);
#2946=LINE('',#18313,#3960);
#2947=LINE('',#18316,#3961);
#2948=LINE('',#18322,#3962);
#2949=LINE('',#18325,#3963);
#2950=LINE('',#18329,#3964);
#2951=LINE('',#18332,#3965);
#2952=LINE('',#18335,#3966);
#2953=LINE('',#18339,#3967);
#2954=LINE('',#18342,#3968);
#2955=LINE('',#18343,#3969);
#2956=LINE('',#18345,#3970);
#2957=LINE('',#18347,#3971);
#2958=LINE('',#18359,#3972);
#2959=LINE('',#18362,#3973);
#2960=LINE('',#18366,#3974);
#2961=LINE('',#18371,#3975);
#2962=LINE('',#18374,#3976);
#2963=LINE('',#18378,#3977);
#2964=LINE('',#18390,#3978);
#2965=LINE('',#18396,#3979);
#2966=LINE('',#18401,#3980);
#2967=LINE('',#18405,#3981);
#2968=LINE('',#18409,#3982);
#2969=LINE('',#18410,#3983);
#2970=LINE('',#18414,#3984);
#2971=LINE('',#18416,#3985);
#2972=LINE('',#18418,#3986);
#2973=LINE('',#18420,#3987);
#2974=LINE('',#18422,#3988);
#2975=LINE('',#18424,#3989);
#2976=LINE('',#18426,#3990);
#2977=LINE('',#18427,#3991);
#2978=LINE('',#18430,#3992);
#2979=LINE('',#18432,#3993);
#2980=LINE('',#18433,#3994);
#2981=LINE('',#18436,#3995);
#2982=LINE('',#18438,#3996);
#2983=LINE('',#18439,#3997);
#2984=LINE('',#18442,#3998);
#2985=LINE('',#18443,#3999);
#2986=LINE('',#18445,#4000);
#2987=LINE('',#18447,#4001);
#2988=LINE('',#18448,#4002);
#2989=LINE('',#18451,#4003);
#2990=LINE('',#18452,#4004);
#2991=LINE('',#18454,#4005);
#2992=LINE('',#18456,#4006);
#2993=LINE('',#18457,#4007);
#2994=LINE('',#18460,#4008);
#2995=LINE('',#18462,#4009);
#2996=LINE('',#18463,#4010);
#2997=LINE('',#18467,#4011);
#2998=LINE('',#18469,#4012);
#2999=LINE('',#18470,#4013);
#3000=LINE('',#18473,#4014);
#3001=LINE('',#18475,#4015);
#3002=LINE('',#18478,#4016);
#3003=LINE('',#18480,#4017);
#3004=LINE('',#18489,#4018);
#3005=LINE('',#18493,#4019);
#3006=LINE('',#18497,#4020);
#3007=LINE('',#18501,#4021);
#3008=LINE('',#18505,#4022);
#3009=LINE('',#18507,#4023);
#3010=LINE('',#18509,#4024);
#3011=LINE('',#18510,#4025);
#3012=LINE('',#18514,#4026);
#3013=LINE('',#18518,#4027);
#3014=LINE('',#18522,#4028);
#3015=LINE('',#18526,#4029);
#3016=LINE('',#18530,#4030);
#3017=LINE('',#18532,#4031);
#3018=LINE('',#18534,#4032);
#3019=LINE('',#18535,#4033);
#3020=LINE('',#18537,#4034);
#3021=LINE('',#18538,#4035);
#3022=LINE('',#18540,#4036);
#3023=LINE('',#18541,#4037);
#3024=LINE('',#18543,#4038);
#3025=LINE('',#18544,#4039);
#3026=LINE('',#18546,#4040);
#3027=LINE('',#18547,#4041);
#3028=LINE('',#18549,#4042);
#3029=LINE('',#18550,#4043);
#3030=LINE('',#18552,#4044);
#3031=LINE('',#18554,#4045);
#3032=LINE('',#18565,#4046);
#3033=LINE('',#18573,#4047);
#3034=LINE('',#18577,#4048);
#3035=LINE('',#18583,#4049);
#3036=LINE('',#18589,#4050);
#3037=LINE('',#18595,#4051);
#3038=LINE('',#18601,#4052);
#3039=LINE('',#18647,#4053);
#3040=LINE('',#18656,#4054);
#3041=LINE('',#18665,#4055);
#3042=LINE('',#18669,#4056);
#3043=LINE('',#18679,#4057);
#3044=LINE('',#18682,#4058);
#3045=LINE('',#18693,#4059);
#3046=LINE('',#18706,#4060);
#3047=LINE('',#18711,#4061);
#3048=LINE('',#18717,#4062);
#3049=LINE('',#18720,#4063);
#3050=LINE('',#18727,#4064);
#3051=LINE('',#18735,#4065);
#3052=LINE('',#18742,#4066);
#3053=LINE('',#18750,#4067);
#3054=LINE('',#18754,#4068);
#3055=LINE('',#18759,#4069);
#3056=LINE('',#18761,#4070);
#3057=LINE('',#18766,#4071);
#3058=LINE('',#18781,#4072);
#3059=LINE('',#18795,#4073);
#3060=LINE('',#18797,#4074);
#3061=VECTOR('',#12311,2.);
#3062=VECTOR('',#12318,2.);
#3063=VECTOR('',#12325,4.);
#3064=VECTOR('',#12332,2.25);
#3065=VECTOR('',#12339,4.);
#3066=VECTOR('',#12346,2.25);
#3067=VECTOR('',#12353,7.00000000000001);
#3068=VECTOR('',#12360,10.);
#3069=VECTOR('',#12367,11.1);
#3070=VECTOR('',#12372,1000.);
#3071=VECTOR('',#12373,1000.);
#3072=VECTOR('',#12374,1000.);
#3073=VECTOR('',#12375,1000.);
#3074=VECTOR('',#12376,1000.);
#3075=VECTOR('',#12377,1000.);
#3076=VECTOR('',#12378,1000.);
#3077=VECTOR('',#12379,1000.);
#3078=VECTOR('',#12380,1000.);
#3079=VECTOR('',#12381,1000.);
#3080=VECTOR('',#12384,1000.);
#3081=VECTOR('',#12385,1000.);
#3082=VECTOR('',#12388,1000.);
#3083=VECTOR('',#12391,1000.);
#3084=VECTOR('',#12392,1000.);
#3085=VECTOR('',#12395,1000.);
#3086=VECTOR('',#12398,1000.);
#3087=VECTOR('',#12399,1000.);
#3088=VECTOR('',#12400,1000.);
#3089=VECTOR('',#12401,1000.);
#3090=VECTOR('',#12404,1000.);
#3091=VECTOR('',#12405,1000.);
#3092=VECTOR('',#12406,1000.);
#3093=VECTOR('',#12407,1000.);
#3094=VECTOR('',#12408,1000.);
#3095=VECTOR('',#12409,1000.);
#3096=VECTOR('',#12410,1000.);
#3097=VECTOR('',#12411,1000.);
#3098=VECTOR('',#12412,1000.);
#3099=VECTOR('',#12413,1000.);
#3100=VECTOR('',#12414,1000.);
#3101=VECTOR('',#12415,1000.);
#3102=VECTOR('',#12416,1000.);
#3103=VECTOR('',#12417,1000.);
#3104=VECTOR('',#12418,1000.);
#3105=VECTOR('',#12421,1000.);
#3106=VECTOR('',#12422,1000.);
#3107=VECTOR('',#12423,1000.);
#3108=VECTOR('',#12426,1000.);
#3109=VECTOR('',#12431,1000.);
#3110=VECTOR('',#12432,1000.);
#3111=VECTOR('',#12433,1000.);
#3112=VECTOR('',#12434,1000.);
#3113=VECTOR('',#12437,1000.);
#3114=VECTOR('',#12438,1000.);
#3115=VECTOR('',#12439,1000.);
#3116=VECTOR('',#12440,1000.);
#3117=VECTOR('',#12441,1000.);
#3118=VECTOR('',#12442,1000.);
#3119=VECTOR('',#12445,1000.);
#3120=VECTOR('',#12446,1000.);
#3121=VECTOR('',#12459,1000.);
#3122=VECTOR('',#12460,1000.);
#3123=VECTOR('',#12463,1000.);
#3124=VECTOR('',#12464,1000.);
#3125=VECTOR('',#12467,1000.);
#3126=VECTOR('',#12468,1000.);
#3127=VECTOR('',#12469,1000.);
#3128=VECTOR('',#12480,1000.);
#3129=VECTOR('',#12481,1000.);
#3130=VECTOR('',#12482,1000.);
#3131=VECTOR('',#12485,1000.);
#3132=VECTOR('',#12486,1000.);
#3133=VECTOR('',#12489,1000.);
#3134=VECTOR('',#12490,1000.);
#3135=VECTOR('',#12493,1000.);
#3136=VECTOR('',#12494,1000.);
#3137=VECTOR('',#12497,1000.);
#3138=VECTOR('',#12498,1000.);
#3139=VECTOR('',#12501,1000.);
#3140=VECTOR('',#12506,1000.);
#3141=VECTOR('',#12507,1000.);
#3142=VECTOR('',#12508,1000.);
#3143=VECTOR('',#12511,1000.);
#3144=VECTOR('',#12512,1000.);
#3145=VECTOR('',#12515,1000.);
#3146=VECTOR('',#12516,1000.);
#3147=VECTOR('',#12519,1000.);
#3148=VECTOR('',#12520,1000.);
#3149=VECTOR('',#12523,1000.);
#3150=VECTOR('',#12524,1000.);
#3151=VECTOR('',#12527,1000.);
#3152=VECTOR('',#12532,1000.);
#3153=VECTOR('',#12535,1000.);
#3154=VECTOR('',#12540,1000.);
#3155=VECTOR('',#12541,1000.);
#3156=VECTOR('',#12552,2.);
#3157=VECTOR('',#12559,2.);
#3158=VECTOR('',#12566,4.);
#3159=VECTOR('',#12573,2.25);
#3160=VECTOR('',#12580,4.);
#3161=VECTOR('',#12587,2.25);
#3162=VECTOR('',#12594,7.00000000000001);
#3163=VECTOR('',#12601,10.);
#3164=VECTOR('',#12608,11.1);
#3165=VECTOR('',#12613,1000.);
#3166=VECTOR('',#12614,1000.);
#3167=VECTOR('',#12615,1000.);
#3168=VECTOR('',#12616,1000.);
#3169=VECTOR('',#12617,1000.);
#3170=VECTOR('',#12618,1000.);
#3171=VECTOR('',#12619,1000.);
#3172=VECTOR('',#12620,1000.);
#3173=VECTOR('',#12621,1000.);
#3174=VECTOR('',#12622,1000.);
#3175=VECTOR('',#12625,1000.);
#3176=VECTOR('',#12626,1000.);
#3177=VECTOR('',#12629,1000.);
#3178=VECTOR('',#12632,1000.);
#3179=VECTOR('',#12633,1000.);
#3180=VECTOR('',#12636,1000.);
#3181=VECTOR('',#12639,1000.);
#3182=VECTOR('',#12640,1000.);
#3183=VECTOR('',#12641,1000.);
#3184=VECTOR('',#12642,1000.);
#3185=VECTOR('',#12645,1000.);
#3186=VECTOR('',#12646,1000.);
#3187=VECTOR('',#12647,1000.);
#3188=VECTOR('',#12648,1000.);
#3189=VECTOR('',#12649,1000.);
#3190=VECTOR('',#12650,1000.);
#3191=VECTOR('',#12651,1000.);
#3192=VECTOR('',#12652,1000.);
#3193=VECTOR('',#12653,1000.);
#3194=VECTOR('',#12654,1000.);
#3195=VECTOR('',#12655,1000.);
#3196=VECTOR('',#12656,1000.);
#3197=VECTOR('',#12657,1000.);
#3198=VECTOR('',#12658,1000.);
#3199=VECTOR('',#12659,1000.);
#3200=VECTOR('',#12662,1000.);
#3201=VECTOR('',#12663,1000.);
#3202=VECTOR('',#12664,1000.);
#3203=VECTOR('',#12669,1000.);
#3204=VECTOR('',#12672,1000.);
#3205=VECTOR('',#12673,1000.);
#3206=VECTOR('',#12674,1000.);
#3207=VECTOR('',#12675,1000.);
#3208=VECTOR('',#12678,1000.);
#3209=VECTOR('',#12679,1000.);
#3210=VECTOR('',#12680,1000.);
#3211=VECTOR('',#12681,1000.);
#3212=VECTOR('',#12682,1000.);
#3213=VECTOR('',#12683,1000.);
#3214=VECTOR('',#12686,1000.);
#3215=VECTOR('',#12687,1000.);
#3216=VECTOR('',#12700,1000.);
#3217=VECTOR('',#12701,1000.);
#3218=VECTOR('',#12704,1000.);
#3219=VECTOR('',#12705,1000.);
#3220=VECTOR('',#12708,1000.);
#3221=VECTOR('',#12709,1000.);
#3222=VECTOR('',#12710,1000.);
#3223=VECTOR('',#12721,1000.);
#3224=VECTOR('',#12722,1000.);
#3225=VECTOR('',#12723,1000.);
#3226=VECTOR('',#12726,1000.);
#3227=VECTOR('',#12727,1000.);
#3228=VECTOR('',#12730,1000.);
#3229=VECTOR('',#12731,1000.);
#3230=VECTOR('',#12734,1000.);
#3231=VECTOR('',#12735,1000.);
#3232=VECTOR('',#12738,1000.);
#3233=VECTOR('',#12739,1000.);
#3234=VECTOR('',#12742,1000.);
#3235=VECTOR('',#12747,1000.);
#3236=VECTOR('',#12748,1000.);
#3237=VECTOR('',#12749,1000.);
#3238=VECTOR('',#12752,1000.);
#3239=VECTOR('',#12753,1000.);
#3240=VECTOR('',#12756,1000.);
#3241=VECTOR('',#12757,1000.);
#3242=VECTOR('',#12760,1000.);
#3243=VECTOR('',#12761,1000.);
#3244=VECTOR('',#12764,1000.);
#3245=VECTOR('',#12765,1000.);
#3246=VECTOR('',#12768,1000.);
#3247=VECTOR('',#12773,1000.);
#3248=VECTOR('',#12776,1000.);
#3249=VECTOR('',#12781,1000.);
#3250=VECTOR('',#12782,1000.);
#3251=VECTOR('',#12793,4.);
#3252=VECTOR('',#12804,2.25);
#3253=VECTOR('',#12811,4.);
#3254=VECTOR('',#12818,2.25);
#3255=VECTOR('',#12825,7.00000000000001);
#3256=VECTOR('',#12832,10.);
#3257=VECTOR('',#12839,11.1);
#3258=VECTOR('',#12844,1000.);
#3259=VECTOR('',#12845,1000.);
#3260=VECTOR('',#12846,1000.);
#3261=VECTOR('',#12849,1000.);
#3262=VECTOR('',#12852,1000.);
#3263=VECTOR('',#12853,1000.);
#3264=VECTOR('',#12856,1000.);
#3265=VECTOR('',#12857,1000.);
#3266=VECTOR('',#12860,1000.);
#3267=VECTOR('',#12861,1000.);
#3268=VECTOR('',#12862,1000.);
#3269=VECTOR('',#12863,1000.);
#3270=VECTOR('',#12864,1000.);
#3271=VECTOR('',#12865,1000.);
#3272=VECTOR('',#12868,1000.);
#3273=VECTOR('',#12869,1000.);
#3274=VECTOR('',#12870,1000.);
#3275=VECTOR('',#12871,1000.);
#3276=VECTOR('',#12878,1000.);
#3277=VECTOR('',#12881,1000.);
#3278=VECTOR('',#12882,1000.);
#3279=VECTOR('',#12883,1000.);
#3280=VECTOR('',#12886,1000.);
#3281=VECTOR('',#12887,1000.);
#3282=VECTOR('',#12888,1000.);
#3283=VECTOR('',#12891,1000.);
#3284=VECTOR('',#12894,1000.);
#3285=VECTOR('',#12895,1000.);
#3286=VECTOR('',#12896,1000.);
#3287=VECTOR('',#12897,1000.);
#3288=VECTOR('',#12898,1000.);
#3289=VECTOR('',#12899,1000.);
#3290=VECTOR('',#12902,1000.);
#3291=VECTOR('',#12903,1000.);
#3292=VECTOR('',#12906,1000.);
#3293=VECTOR('',#12911,1000.);
#3294=VECTOR('',#12912,1000.);
#3295=VECTOR('',#12913,1000.);
#3296=VECTOR('',#12930,1000.);
#3297=VECTOR('',#12931,1000.);
#3298=VECTOR('',#12932,1000.);
#3299=VECTOR('',#12937,1000.);
#3300=VECTOR('',#12940,1000.);
#3301=VECTOR('',#12941,1000.);
#3302=VECTOR('',#12944,1000.);
#3303=VECTOR('',#12945,1000.);
#3304=VECTOR('',#12948,1000.);
#3305=VECTOR('',#12949,1000.);
#3306=VECTOR('',#12958,1000.);
#3307=VECTOR('',#12959,1000.);
#3308=VECTOR('',#12970,4.);
#3309=VECTOR('',#12981,2.25);
#3310=VECTOR('',#12988,4.);
#3311=VECTOR('',#12995,2.25);
#3312=VECTOR('',#13002,7.00000000000001);
#3313=VECTOR('',#13009,10.);
#3314=VECTOR('',#13016,11.1);
#3315=VECTOR('',#13021,1000.);
#3316=VECTOR('',#13022,1000.);
#3317=VECTOR('',#13025,1000.);
#3318=VECTOR('',#13026,1000.);
#3319=VECTOR('',#13029,1000.);
#3320=VECTOR('',#13030,1000.);
#3321=VECTOR('',#13031,1000.);
#3322=VECTOR('',#13034,1000.);
#3323=VECTOR('',#13037,1000.);
#3324=VECTOR('',#13038,1000.);
#3325=VECTOR('',#13039,1000.);
#3326=VECTOR('',#13040,1000.);
#3327=VECTOR('',#13041,1000.);
#3328=VECTOR('',#13042,1000.);
#3329=VECTOR('',#13045,1000.);
#3330=VECTOR('',#13046,1000.);
#3331=VECTOR('',#13047,1000.);
#3332=VECTOR('',#13048,1000.);
#3333=VECTOR('',#13053,1000.);
#3334=VECTOR('',#13058,1000.);
#3335=VECTOR('',#13059,1000.);
#3336=VECTOR('',#13060,1000.);
#3337=VECTOR('',#13063,1000.);
#3338=VECTOR('',#13064,1000.);
#3339=VECTOR('',#13065,1000.);
#3340=VECTOR('',#13066,1000.);
#3341=VECTOR('',#13067,1000.);
#3342=VECTOR('',#13068,1000.);
#3343=VECTOR('',#13069,1000.);
#3344=VECTOR('',#13072,1000.);
#3345=VECTOR('',#13075,1000.);
#3346=VECTOR('',#13076,1000.);
#3347=VECTOR('',#13079,1000.);
#3348=VECTOR('',#13080,1000.);
#3349=VECTOR('',#13083,1000.);
#3350=VECTOR('',#13084,1000.);
#3351=VECTOR('',#13085,1000.);
#3352=VECTOR('',#13086,1000.);
#3353=VECTOR('',#13107,1000.);
#3354=VECTOR('',#13108,1000.);
#3355=VECTOR('',#13109,1000.);
#3356=VECTOR('',#13112,1000.);
#3357=VECTOR('',#13113,1000.);
#3358=VECTOR('',#13116,1000.);
#3359=VECTOR('',#13121,1000.);
#3360=VECTOR('',#13122,1000.);
#3361=VECTOR('',#13125,1000.);
#3362=VECTOR('',#13126,1000.);
#3363=VECTOR('',#13135,1000.);
#3364=VECTOR('',#13136,1000.);
#3365=VECTOR('',#13147,3.);
#3366=VECTOR('',#13154,3.);
#3367=VECTOR('',#13161,3.25);
#3368=VECTOR('',#13168,3.25);
#3369=VECTOR('',#13175,2.25);
#3370=VECTOR('',#13182,1.75);
#3371=VECTOR('',#13189,1.75);
#3372=VECTOR('',#13196,3.);
#3373=VECTOR('',#13203,1.5);
#3374=VECTOR('',#13210,1.5);
#3375=VECTOR('',#13215,1000.);
#3376=VECTOR('',#13216,1000.);
#3377=VECTOR('',#13217,1000.);
#3378=VECTOR('',#13218,1000.);
#3379=VECTOR('',#13221,1000.);
#3380=VECTOR('',#13222,1000.);
#3381=VECTOR('',#13223,1000.);
#3382=VECTOR('',#13224,1000.);
#3383=VECTOR('',#13227,1000.);
#3384=VECTOR('',#13228,1000.);
#3385=VECTOR('',#13229,1000.);
#3386=VECTOR('',#13230,1000.);
#3387=VECTOR('',#13245,1000.);
#3388=VECTOR('',#13246,1000.);
#3389=VECTOR('',#13247,1000.);
#3390=VECTOR('',#13248,1000.);
#3391=VECTOR('',#13253,1000.);
#3392=VECTOR('',#13258,1000.);
#3393=VECTOR('',#13259,1000.);
#3394=VECTOR('',#13260,1000.);
#3395=VECTOR('',#13265,1000.);
#3396=VECTOR('',#13270,1000.);
#3397=VECTOR('',#13271,1000.);
#3398=VECTOR('',#13272,1000.);
#3399=VECTOR('',#13277,1000.);
#3400=VECTOR('',#13282,1000.);
#3401=VECTOR('',#13283,1000.);
#3402=VECTOR('',#13284,1000.);
#3403=VECTOR('',#13293,1000.);
#3404=VECTOR('',#13294,1000.);
#3405=VECTOR('',#13295,1000.);
#3406=VECTOR('',#13296,1000.);
#3407=VECTOR('',#13299,1000.);
#3408=VECTOR('',#13300,1000.);
#3409=VECTOR('',#13301,1000.);
#3410=VECTOR('',#13302,1000.);
#3411=VECTOR('',#13305,1000.);
#3412=VECTOR('',#13306,1000.);
#3413=VECTOR('',#13307,1000.);
#3414=VECTOR('',#13308,1000.);
#3415=VECTOR('',#13311,1000.);
#3416=VECTOR('',#13312,1000.);
#3417=VECTOR('',#13313,1000.);
#3418=VECTOR('',#13314,1000.);
#3419=VECTOR('',#13317,1000.);
#3420=VECTOR('',#13318,1000.);
#3421=VECTOR('',#13319,1000.);
#3422=VECTOR('',#13320,1000.);
#3423=VECTOR('',#13409,7.);
#3424=VECTOR('',#13414,5.);
#3425=VECTOR('',#13419,7.);
#3426=VECTOR('',#13428,1000.);
#3427=VECTOR('',#13431,1000.);
#3428=VECTOR('',#13436,1000.);
#3429=VECTOR('',#13439,1000.);
#3430=VECTOR('',#13442,1000.);
#3431=VECTOR('',#13443,1000.);
#3432=VECTOR('',#13446,1000.);
#3433=VECTOR('',#13449,1000.);
#3434=VECTOR('',#13458,4.);
#3435=VECTOR('',#13499,12.);
#3436=VECTOR('',#13504,10.);
#3437=VECTOR('',#13509,12.);
#3438=VECTOR('',#13534,2.);
#3439=VECTOR('',#13539,1.);
#3440=VECTOR('',#13546,1.);
#3441=VECTOR('',#13553,1.5);
#3442=VECTOR('',#13560,1.5);
#3443=VECTOR('',#13567,1.);
#3444=VECTOR('',#13574,2.75);
#3445=VECTOR('',#13577,1000.);
#3446=VECTOR('',#13580,1000.);
#3447=VECTOR('',#13583,1000.);
#3448=VECTOR('',#13586,1000.);
#3449=VECTOR('',#13599,1000.);
#3450=VECTOR('',#13602,1000.);
#3451=VECTOR('',#13607,1000.);
#3452=VECTOR('',#13612,1000.);
#3453=VECTOR('',#13617,2.75);
#3454=VECTOR('',#13620,1000.);
#3455=VECTOR('',#13623,1000.);
#3456=VECTOR('',#13626,1000.);
#3457=VECTOR('',#13629,1000.);
#3458=VECTOR('',#13634,1000.);
#3459=VECTOR('',#13635,1000.);
#3460=VECTOR('',#13638,1000.);
#3461=VECTOR('',#13641,1000.);
#3462=VECTOR('',#13642,1000.);
#3463=VECTOR('',#13643,1000.);
#3464=VECTOR('',#13644,1000.);
#3465=VECTOR('',#13647,1000.);
#3466=VECTOR('',#13648,1000.);
#3467=VECTOR('',#13649,1000.);
#3468=VECTOR('',#13650,1000.);
#3469=VECTOR('',#13651,1000.);
#3470=VECTOR('',#13652,1000.);
#3471=VECTOR('',#13653,1000.);
#3472=VECTOR('',#13656,1000.);
#3473=VECTOR('',#13657,1000.);
#3474=VECTOR('',#13662,1000.);
#3475=VECTOR('',#13663,1000.);
#3476=VECTOR('',#13666,1000.);
#3477=VECTOR('',#13673,1000.);
#3478=VECTOR('',#13676,1000.);
#3479=VECTOR('',#13679,1000.);
#3480=VECTOR('',#13680,1000.);
#3481=VECTOR('',#13681,1000.);
#3482=VECTOR('',#13682,1000.);
#3483=VECTOR('',#13685,1000.);
#3484=VECTOR('',#13688,1000.);
#3485=VECTOR('',#13689,1000.);
#3486=VECTOR('',#13698,1000.);
#3487=VECTOR('',#13701,1000.);
#3488=VECTOR('',#13708,1000.);
#3489=VECTOR('',#13709,1000.);
#3490=VECTOR('',#13712,1000.);
#3491=VECTOR('',#13715,1000.);
#3492=VECTOR('',#13720,1000.);
#3493=VECTOR('',#13721,1000.);
#3494=VECTOR('',#13730,1000.);
#3495=VECTOR('',#13731,1000.);
#3496=VECTOR('',#13734,1000.);
#3497=VECTOR('',#13739,1000.);
#3498=VECTOR('',#13744,1000.);
#3499=VECTOR('',#13749,1000.);
#3500=VECTOR('',#13754,1000.);
#3501=VECTOR('',#13755,1000.);
#3502=VECTOR('',#13756,1000.);
#3503=VECTOR('',#13759,1000.);
#3504=VECTOR('',#13760,1000.);
#3505=VECTOR('',#13763,1000.);
#3506=VECTOR('',#13764,1000.);
#3507=VECTOR('',#13767,1000.);
#3508=VECTOR('',#13778,1000.);
#3509=VECTOR('',#13781,1000.);
#3510=VECTOR('',#13786,1000.);
#3511=VECTOR('',#13789,1000.);
#3512=VECTOR('',#13792,1000.);
#3513=VECTOR('',#13795,1000.);
#3514=VECTOR('',#13796,1000.);
#3515=VECTOR('',#13797,1000.);
#3516=VECTOR('',#13802,1000.);
#3517=VECTOR('',#13805,1000.);
#3518=VECTOR('',#13806,1000.);
#3519=VECTOR('',#13809,1000.);
#3520=VECTOR('',#13812,1000.);
#3521=VECTOR('',#13815,1000.);
#3522=VECTOR('',#13820,1000.);
#3523=VECTOR('',#13823,1000.);
#3524=VECTOR('',#13832,1000.);
#3525=VECTOR('',#13835,1000.);
#3526=VECTOR('',#13840,1000.);
#3527=VECTOR('',#13843,1000.);
#3528=VECTOR('',#13846,1000.);
#3529=VECTOR('',#13847,1000.);
#3530=VECTOR('',#13848,1000.);
#3531=VECTOR('',#13851,1000.);
#3532=VECTOR('',#13852,1000.);
#3533=VECTOR('',#13853,1000.);
#3534=VECTOR('',#13856,1000.);
#3535=VECTOR('',#13857,1000.);
#3536=VECTOR('',#13860,1000.);
#3537=VECTOR('',#13863,1000.);
#3538=VECTOR('',#13864,1000.);
#3539=VECTOR('',#13865,1000.);
#3540=VECTOR('',#13866,1000.);
#3541=VECTOR('',#13867,1000.);
#3542=VECTOR('',#13868,1000.);
#3543=VECTOR('',#13871,1000.);
#3544=VECTOR('',#13874,1000.);
#3545=VECTOR('',#13877,1000.);
#3546=VECTOR('',#13880,1000.);
#3547=VECTOR('',#13883,1000.);
#3548=VECTOR('',#13888,1000.);
#3549=VECTOR('',#13891,1000.);
#3550=VECTOR('',#13894,1000.);
#3551=VECTOR('',#13897,1000.);
#3552=VECTOR('',#13906,1000.);
#3553=VECTOR('',#13909,1000.);
#3554=VECTOR('',#13912,1000.);
#3555=VECTOR('',#13913,1000.);
#3556=VECTOR('',#13914,1000.);
#3557=VECTOR('',#13915,1000.);
#3558=VECTOR('',#13916,1000.);
#3559=VECTOR('',#13919,1000.);
#3560=VECTOR('',#13922,1000.);
#3561=VECTOR('',#13925,1000.);
#3562=VECTOR('',#13928,1000.);
#3563=VECTOR('',#13931,1000.);
#3564=VECTOR('',#13934,1000.);
#3565=VECTOR('',#13937,1000.);
#3566=VECTOR('',#13940,1000.);
#3567=VECTOR('',#13943,1000.);
#3568=VECTOR('',#13946,1000.);
#3569=VECTOR('',#13949,1000.);
#3570=VECTOR('',#13950,1000.);
#3571=VECTOR('',#13951,1000.);
#3572=VECTOR('',#13952,1000.);
#3573=VECTOR('',#13953,1000.);
#3574=VECTOR('',#13954,1000.);
#3575=VECTOR('',#13955,1000.);
#3576=VECTOR('',#13956,1000.);
#3577=VECTOR('',#13959,1000.);
#3578=VECTOR('',#13962,1000.);
#3579=VECTOR('',#13965,1000.);
#3580=VECTOR('',#13968,1000.);
#3581=VECTOR('',#13971,1000.);
#3582=VECTOR('',#13974,1000.);
#3583=VECTOR('',#13977,1000.);
#3584=VECTOR('',#13980,1000.);
#3585=VECTOR('',#13983,1000.);
#3586=VECTOR('',#13986,1000.);
#3587=VECTOR('',#13989,1000.);
#3588=VECTOR('',#13990,1000.);
#3589=VECTOR('',#13991,1000.);
#3590=VECTOR('',#13992,1000.);
#3591=VECTOR('',#13993,1000.);
#3592=VECTOR('',#13994,1000.);
#3593=VECTOR('',#13995,1000.);
#3594=VECTOR('',#13996,1000.);
#3595=VECTOR('',#13999,1000.);
#3596=VECTOR('',#14002,1000.);
#3597=VECTOR('',#14005,1000.);
#3598=VECTOR('',#14008,1000.);
#3599=VECTOR('',#14011,1000.);
#3600=VECTOR('',#14014,1000.);
#3601=VECTOR('',#14017,1000.);
#3602=VECTOR('',#14020,1000.);
#3603=VECTOR('',#14023,1000.);
#3604=VECTOR('',#14026,1000.);
#3605=VECTOR('',#14029,1000.);
#3606=VECTOR('',#14030,1000.);
#3607=VECTOR('',#14031,1000.);
#3608=VECTOR('',#14032,1000.);
#3609=VECTOR('',#14033,1000.);
#3610=VECTOR('',#14034,1000.);
#3611=VECTOR('',#14035,1000.);
#3612=VECTOR('',#14036,1000.);
#3613=VECTOR('',#14039,1000.);
#3614=VECTOR('',#14042,1000.);
#3615=VECTOR('',#14045,1000.);
#3616=VECTOR('',#14048,1000.);
#3617=VECTOR('',#14051,1000.);
#3618=VECTOR('',#14054,1000.);
#3619=VECTOR('',#14057,1000.);
#3620=VECTOR('',#14060,1000.);
#3621=VECTOR('',#14063,1000.);
#3622=VECTOR('',#14066,1000.);
#3623=VECTOR('',#14069,1000.);
#3624=VECTOR('',#14070,1000.);
#3625=VECTOR('',#14071,1000.);
#3626=VECTOR('',#14072,1000.);
#3627=VECTOR('',#14075,1000.);
#3628=VECTOR('',#14078,1000.);
#3629=VECTOR('',#14081,1000.);
#3630=VECTOR('',#14084,1000.);
#3631=VECTOR('',#14087,1000.);
#3632=VECTOR('',#14090,1000.);
#3633=VECTOR('',#14093,1000.);
#3634=VECTOR('',#14096,1000.);
#3635=VECTOR('',#14099,1000.);
#3636=VECTOR('',#14102,1000.);
#3637=VECTOR('',#14103,1000.);
#3638=VECTOR('',#14106,1000.);
#3639=VECTOR('',#14109,1000.);
#3640=VECTOR('',#14112,1000.);
#3641=VECTOR('',#14115,1000.);
#3642=VECTOR('',#14118,1000.);
#3643=VECTOR('',#14121,1000.);
#3644=VECTOR('',#14124,1000.);
#3645=VECTOR('',#14127,1000.);
#3646=VECTOR('',#14130,1000.);
#3647=VECTOR('',#14133,1000.);
#3648=VECTOR('',#14136,1000.);
#3649=VECTOR('',#14139,1000.);
#3650=VECTOR('',#14144,1000.);
#3651=VECTOR('',#14145,1000.);
#3652=VECTOR('',#14146,1000.);
#3653=VECTOR('',#14147,1000.);
#3654=VECTOR('',#14150,1000.);
#3655=VECTOR('',#14153,1000.);
#3656=VECTOR('',#14156,1000.);
#3657=VECTOR('',#14159,1000.);
#3658=VECTOR('',#14162,1000.);
#3659=VECTOR('',#14165,1000.);
#3660=VECTOR('',#14168,1000.);
#3661=VECTOR('',#14171,1000.);
#3662=VECTOR('',#14174,1000.);
#3663=VECTOR('',#14177,1000.);
#3664=VECTOR('',#14180,1000.);
#3665=VECTOR('',#14181,1000.);
#3666=VECTOR('',#14182,1000.);
#3667=VECTOR('',#14183,1000.);
#3668=VECTOR('',#14184,1000.);
#3669=VECTOR('',#14185,1000.);
#3670=VECTOR('',#14186,1000.);
#3671=VECTOR('',#14187,1000.);
#3672=VECTOR('',#14190,1000.);
#3673=VECTOR('',#14193,1000.);
#3674=VECTOR('',#14196,1000.);
#3675=VECTOR('',#14199,1000.);
#3676=VECTOR('',#14202,1000.);
#3677=VECTOR('',#14205,1000.);
#3678=VECTOR('',#14208,1000.);
#3679=VECTOR('',#14211,1000.);
#3680=VECTOR('',#14214,1000.);
#3681=VECTOR('',#14217,1000.);
#3682=VECTOR('',#14220,1000.);
#3683=VECTOR('',#14221,1000.);
#3684=VECTOR('',#14222,1000.);
#3685=VECTOR('',#14223,1000.);
#3686=VECTOR('',#14224,1000.);
#3687=VECTOR('',#14225,1000.);
#3688=VECTOR('',#14226,1000.);
#3689=VECTOR('',#14227,1000.);
#3690=VECTOR('',#14230,1000.);
#3691=VECTOR('',#14233,1000.);
#3692=VECTOR('',#14236,1000.);
#3693=VECTOR('',#14239,1000.);
#3694=VECTOR('',#14242,1000.);
#3695=VECTOR('',#14245,1000.);
#3696=VECTOR('',#14248,1000.);
#3697=VECTOR('',#14251,1000.);
#3698=VECTOR('',#14254,1000.);
#3699=VECTOR('',#14257,1000.);
#3700=VECTOR('',#14260,1000.);
#3701=VECTOR('',#14261,1000.);
#3702=VECTOR('',#14262,1000.);
#3703=VECTOR('',#14263,1000.);
#3704=VECTOR('',#14264,1000.);
#3705=VECTOR('',#14265,1000.);
#3706=VECTOR('',#14266,1000.);
#3707=VECTOR('',#14267,1000.);
#3708=VECTOR('',#14270,1000.);
#3709=VECTOR('',#14273,1000.);
#3710=VECTOR('',#14276,1000.);
#3711=VECTOR('',#14279,1000.);
#3712=VECTOR('',#14282,1000.);
#3713=VECTOR('',#14285,1000.);
#3714=VECTOR('',#14288,1000.);
#3715=VECTOR('',#14291,1000.);
#3716=VECTOR('',#14294,1000.);
#3717=VECTOR('',#14297,1000.);
#3718=VECTOR('',#14300,1000.);
#3719=VECTOR('',#14301,1000.);
#3720=VECTOR('',#14302,1000.);
#3721=VECTOR('',#14303,1000.);
#3722=VECTOR('',#14306,1000.);
#3723=VECTOR('',#14309,1000.);
#3724=VECTOR('',#14312,1000.);
#3725=VECTOR('',#14315,1000.);
#3726=VECTOR('',#14318,1000.);
#3727=VECTOR('',#14321,1000.);
#3728=VECTOR('',#14324,1000.);
#3729=VECTOR('',#14327,1000.);
#3730=VECTOR('',#14330,1000.);
#3731=VECTOR('',#14333,1000.);
#3732=VECTOR('',#14336,1000.);
#3733=VECTOR('',#14339,1000.);
#3734=VECTOR('',#14342,1000.);
#3735=VECTOR('',#14345,1000.);
#3736=VECTOR('',#14348,1000.);
#3737=VECTOR('',#14351,1000.);
#3738=VECTOR('',#14354,1000.);
#3739=VECTOR('',#14357,1000.);
#3740=VECTOR('',#14358,1000.);
#3741=VECTOR('',#14361,1000.);
#3742=VECTOR('',#14364,1000.);
#3743=VECTOR('',#14367,1000.);
#3744=VECTOR('',#14370,1000.);
#3745=VECTOR('',#14373,1000.);
#3746=VECTOR('',#14376,1000.);
#3747=VECTOR('',#14377,1000.);
#3748=VECTOR('',#14380,1000.);
#3749=VECTOR('',#14383,1000.);
#3750=VECTOR('',#14386,1000.);
#3751=VECTOR('',#14389,1000.);
#3752=VECTOR('',#14392,1000.);
#3753=VECTOR('',#14395,1000.);
#3754=VECTOR('',#14398,1000.);
#3755=VECTOR('',#14401,1000.);
#3756=VECTOR('',#14404,1000.);
#3757=VECTOR('',#14407,1000.);
#3758=VECTOR('',#14410,1000.);
#3759=VECTOR('',#14413,1000.);
#3760=VECTOR('',#14416,1000.);
#3761=VECTOR('',#14419,1000.);
#3762=VECTOR('',#14422,1000.);
#3763=VECTOR('',#14425,1000.);
#3764=VECTOR('',#14428,1000.);
#3765=VECTOR('',#14431,1000.);
#3766=VECTOR('',#14434,1000.);
#3767=VECTOR('',#14437,1000.);
#3768=VECTOR('',#14440,1000.);
#3769=VECTOR('',#14443,1000.);
#3770=VECTOR('',#14446,1000.);
#3771=VECTOR('',#14449,1000.);
#3772=VECTOR('',#14452,1000.);
#3773=VECTOR('',#14455,1000.);
#3774=VECTOR('',#14458,1000.);
#3775=VECTOR('',#14461,1000.);
#3776=VECTOR('',#14464,1000.);
#3777=VECTOR('',#14467,1000.);
#3778=VECTOR('',#14470,1000.);
#3779=VECTOR('',#14473,1000.);
#3780=VECTOR('',#14476,1000.);
#3781=VECTOR('',#14479,1000.);
#3782=VECTOR('',#14482,1000.);
#3783=VECTOR('',#14485,1000.);
#3784=VECTOR('',#14488,1000.);
#3785=VECTOR('',#14491,1000.);
#3786=VECTOR('',#14494,1000.);
#3787=VECTOR('',#14497,1000.);
#3788=VECTOR('',#14500,1000.);
#3789=VECTOR('',#14503,1000.);
#3790=VECTOR('',#14506,1000.);
#3791=VECTOR('',#14509,1000.);
#3792=VECTOR('',#14512,1000.);
#3793=VECTOR('',#14515,1000.);
#3794=VECTOR('',#14518,1000.);
#3795=VECTOR('',#14521,1000.);
#3796=VECTOR('',#14524,1000.);
#3797=VECTOR('',#14527,1000.);
#3798=VECTOR('',#14530,1000.);
#3799=VECTOR('',#14533,1000.);
#3800=VECTOR('',#14536,1000.);
#3801=VECTOR('',#14539,1000.);
#3802=VECTOR('',#14542,1000.);
#3803=VECTOR('',#14545,1000.);
#3804=VECTOR('',#14548,1000.);
#3805=VECTOR('',#14551,1000.);
#3806=VECTOR('',#14554,1000.);
#3807=VECTOR('',#14557,1000.);
#3808=VECTOR('',#14560,1000.);
#3809=VECTOR('',#14563,1000.);
#3810=VECTOR('',#14566,1000.);
#3811=VECTOR('',#14569,1000.);
#3812=VECTOR('',#14572,1000.);
#3813=VECTOR('',#14575,1000.);
#3814=VECTOR('',#14578,1000.);
#3815=VECTOR('',#14581,1000.);
#3816=VECTOR('',#14584,1000.);
#3817=VECTOR('',#14587,1000.);
#3818=VECTOR('',#14590,1000.);
#3819=VECTOR('',#14593,1000.);
#3820=VECTOR('',#14596,1000.);
#3821=VECTOR('',#14599,1000.);
#3822=VECTOR('',#14602,1000.);
#3823=VECTOR('',#14605,1000.);
#3824=VECTOR('',#14608,1000.);
#3825=VECTOR('',#14611,1000.);
#3826=VECTOR('',#14614,1000.);
#3827=VECTOR('',#14617,1000.);
#3828=VECTOR('',#14620,1000.);
#3829=VECTOR('',#14623,1000.);
#3830=VECTOR('',#14626,1000.);
#3831=VECTOR('',#14629,1000.);
#3832=VECTOR('',#14632,1000.);
#3833=VECTOR('',#14635,1000.);
#3834=VECTOR('',#14638,1000.);
#3835=VECTOR('',#14641,1000.);
#3836=VECTOR('',#14644,1000.);
#3837=VECTOR('',#14647,1000.);
#3838=VECTOR('',#14650,1000.);
#3839=VECTOR('',#14653,1000.);
#3840=VECTOR('',#14656,1000.);
#3841=VECTOR('',#14659,1000.);
#3842=VECTOR('',#14662,1000.);
#3843=VECTOR('',#14665,1000.);
#3844=VECTOR('',#14668,1000.);
#3845=VECTOR('',#14671,1000.);
#3846=VECTOR('',#14674,1000.);
#3847=VECTOR('',#14677,1000.);
#3848=VECTOR('',#14680,1000.);
#3849=VECTOR('',#14683,1000.);
#3850=VECTOR('',#14686,1000.);
#3851=VECTOR('',#14689,1000.);
#3852=VECTOR('',#14692,1000.);
#3853=VECTOR('',#14695,1000.);
#3854=VECTOR('',#14698,1000.);
#3855=VECTOR('',#14701,1000.);
#3856=VECTOR('',#14704,1000.);
#3857=VECTOR('',#14707,1000.);
#3858=VECTOR('',#14710,1000.);
#3859=VECTOR('',#14713,1000.);
#3860=VECTOR('',#14716,1000.);
#3861=VECTOR('',#14719,1000.);
#3862=VECTOR('',#14724,1000.);
#3863=VECTOR('',#14725,1000.);
#3864=VECTOR('',#14728,1000.);
#3865=VECTOR('',#14731,1000.);
#3866=VECTOR('',#14734,1000.);
#3867=VECTOR('',#14737,1000.);
#3868=VECTOR('',#14740,1000.);
#3869=VECTOR('',#14743,1000.);
#3870=VECTOR('',#14748,1000.);
#3871=VECTOR('',#14749,1000.);
#3872=VECTOR('',#14752,1000.);
#3873=VECTOR('',#14755,1000.);
#3874=VECTOR('',#14760,1000.);
#3875=VECTOR('',#14763,1000.);
#3876=VECTOR('',#14766,1000.);
#3877=VECTOR('',#14769,1000.);
#3878=VECTOR('',#14772,1000.);
#3879=VECTOR('',#14775,1000.);
#3880=VECTOR('',#14778,1000.);
#3881=VECTOR('',#14781,1000.);
#3882=VECTOR('',#14784,1000.);
#3883=VECTOR('',#14787,1000.);
#3884=VECTOR('',#14792,1000.);
#3885=VECTOR('',#14793,1000.);
#3886=VECTOR('',#14796,1000.);
#3887=VECTOR('',#14799,1000.);
#3888=VECTOR('',#14802,1000.);
#3889=VECTOR('',#14805,1000.);
#3890=VECTOR('',#14808,1000.);
#3891=VECTOR('',#14811,1000.);
#3892=VECTOR('',#14816,1000.);
#3893=VECTOR('',#14817,1000.);
#3894=VECTOR('',#14820,1000.);
#3895=VECTOR('',#14823,1000.);
#3896=VECTOR('',#14826,1000.);
#3897=VECTOR('',#14829,1000.);
#3898=VECTOR('',#14832,1000.);
#3899=VECTOR('',#14835,1000.);
#3900=VECTOR('',#14840,1000.);
#3901=VECTOR('',#14841,1000.);
#3902=VECTOR('',#14844,1000.);
#3903=VECTOR('',#14847,1000.);
#3904=VECTOR('',#14850,1000.);
#3905=VECTOR('',#14853,1000.);
#3906=VECTOR('',#14856,1000.);
#3907=VECTOR('',#14859,1000.);
#3908=VECTOR('',#14868,2.25);
#3909=VECTOR('',#14875,2.25);
#3910=VECTOR('',#14880,1000.);
#3911=VECTOR('',#14881,1000.);
#3912=VECTOR('',#14882,1000.);
#3913=VECTOR('',#14883,1000.);
#3914=VECTOR('',#14888,1000.);
#3915=VECTOR('',#14889,1000.);
#3916=VECTOR('',#14890,1000.);
#3917=VECTOR('',#14891,1000.);
#3918=VECTOR('',#14896,1000.);
#3919=VECTOR('',#14897,1000.);
#3920=VECTOR('',#14898,1000.);
#3921=VECTOR('',#14901,1000.);
#3922=VECTOR('',#14904,1000.);
#3923=VECTOR('',#14905,1000.);
#3924=VECTOR('',#14906,1000.);
#3925=VECTOR('',#14907,1000.);
#3926=VECTOR('',#14908,1000.);
#3927=VECTOR('',#14909,1000.);
#3928=VECTOR('',#14914,1000.);
#3929=VECTOR('',#14915,1000.);
#3930=VECTOR('',#14916,1000.);
#3931=VECTOR('',#14921,1000.);
#3932=VECTOR('',#14922,1000.);
#3933=VECTOR('',#14923,1000.);
#3934=VECTOR('',#14924,1000.);
#3935=VECTOR('',#14925,1000.);
#3936=VECTOR('',#14926,1000.);
#3937=VECTOR('',#14927,1000.);
#3938=VECTOR('',#14928,1000.);
#3939=VECTOR('',#14931,1000.);
#3940=VECTOR('',#14932,1000.);
#3941=VECTOR('',#14933,1000.);
#3942=VECTOR('',#14936,1000.);
#3943=VECTOR('',#14939,1000.);
#3944=VECTOR('',#14940,1000.);
#3945=VECTOR('',#14941,1000.);
#3946=VECTOR('',#14942,1000.);
#3947=VECTOR('',#14943,1000.);
#3948=VECTOR('',#14944,1000.);
#3949=VECTOR('',#14947,1000.);
#3950=VECTOR('',#14952,1000.);
#3951=VECTOR('',#14953,1000.);
#3952=VECTOR('',#14956,1000.);
#3953=VECTOR('',#14957,1000.);
#3954=VECTOR('',#14958,1000.);
#3955=VECTOR('',#14959,1000.);
#3956=VECTOR('',#14960,1000.);
#3957=VECTOR('',#14961,1000.);
#3958=VECTOR('',#14962,1000.);
#3959=VECTOR('',#14963,1000.);
#3960=VECTOR('',#14968,1000.);
#3961=VECTOR('',#14973,1000.);
#3962=VECTOR('',#14978,1000.);
#3963=VECTOR('',#14981,1000.);
#3964=VECTOR('',#14988,1000.);
#3965=VECTOR('',#14993,1000.);
#3966=VECTOR('',#14994,1000.);
#3967=VECTOR('',#14997,1000.);
#3968=VECTOR('',#15002,1000.);
#3969=VECTOR('',#15003,1000.);
#3970=VECTOR('',#15006,1000.);
#3971=VECTOR('',#15009,1000.);
#3972=VECTOR('',#15030,1000.);
#3973=VECTOR('',#15033,1000.);
#3974=VECTOR('',#15040,1000.);
#3975=VECTOR('',#15047,1000.);
#3976=VECTOR('',#15050,1000.);
#3977=VECTOR('',#15057,1000.);
#3978=VECTOR('',#15076,3.99999999999999);
#3979=VECTOR('',#15083,2.15);
#3980=VECTOR('',#15088,1000.);
#3981=VECTOR('',#15091,1000.);
#3982=VECTOR('',#15094,1000.);
#3983=VECTOR('',#15095,1000.);
#3984=VECTOR('',#15098,1000.);
#3985=VECTOR('',#15099,1000.);
#3986=VECTOR('',#15100,1000.);
#3987=VECTOR('',#15101,1000.);
#3988=VECTOR('',#15102,1000.);
#3989=VECTOR('',#15103,1000.);
#3990=VECTOR('',#15104,1000.);
#3991=VECTOR('',#15105,1000.);
#3992=VECTOR('',#15108,1000.);
#3993=VECTOR('',#15109,1000.);
#3994=VECTOR('',#15110,1000.);
#3995=VECTOR('',#15113,1000.);
#3996=VECTOR('',#15114,1000.);
#3997=VECTOR('',#15115,1000.);
#3998=VECTOR('',#15118,1000.);
#3999=VECTOR('',#15119,1000.);
#4000=VECTOR('',#15120,1000.);
#4001=VECTOR('',#15121,1000.);
#4002=VECTOR('',#15122,1000.);
#4003=VECTOR('',#15125,1000.);
#4004=VECTOR('',#15126,1000.);
#4005=VECTOR('',#15127,1000.);
#4006=VECTOR('',#15128,1000.);
#4007=VECTOR('',#15129,1000.);
#4008=VECTOR('',#15132,1000.);
#4009=VECTOR('',#15133,1000.);
#4010=VECTOR('',#15134,1000.);
#4011=VECTOR('',#15139,1000.);
#4012=VECTOR('',#15140,1000.);
#4013=VECTOR('',#15141,1000.);
#4014=VECTOR('',#15146,1000.);
#4015=VECTOR('',#15149,1000.);
#4016=VECTOR('',#15154,1000.);
#4017=VECTOR('',#15157,1000.);
#4018=VECTOR('',#15170,1000.);
#4019=VECTOR('',#15173,1000.);
#4020=VECTOR('',#15176,1000.);
#4021=VECTOR('',#15179,1000.);
#4022=VECTOR('',#15182,1000.);
#4023=VECTOR('',#15183,1000.);
#4024=VECTOR('',#15184,1000.);
#4025=VECTOR('',#15185,1000.);
#4026=VECTOR('',#15188,1000.);
#4027=VECTOR('',#15191,1000.);
#4028=VECTOR('',#15194,1000.);
#4029=VECTOR('',#15197,1000.);
#4030=VECTOR('',#15200,1000.);
#4031=VECTOR('',#15201,1000.);
#4032=VECTOR('',#15202,1000.);
#4033=VECTOR('',#15203,1000.);
#4034=VECTOR('',#15206,1000.);
#4035=VECTOR('',#15207,1000.);
#4036=VECTOR('',#15210,1000.);
#4037=VECTOR('',#15211,1000.);
#4038=VECTOR('',#15214,1000.);
#4039=VECTOR('',#15215,1000.);
#4040=VECTOR('',#15218,1000.);
#4041=VECTOR('',#15219,1000.);
#4042=VECTOR('',#15222,1000.);
#4043=VECTOR('',#15223,1000.);
#4044=VECTOR('',#15226,1000.);
#4045=VECTOR('',#15229,1000.);
#4046=VECTOR('',#15246,9.);
#4047=VECTOR('',#15255,12.7);
#4048=VECTOR('',#15260,12.7);
#4049=VECTOR('',#15267,6.2);
#4050=VECTOR('',#15274,6.2);
#4051=VECTOR('',#15281,4.2);
#4052=VECTOR('',#15288,4.2);
#4053=VECTOR('',#15345,11.);
#4054=VECTOR('',#15356,9.6);
#4055=VECTOR('',#15369,8.8);
#4056=VECTOR('',#15374,8.8);
#4057=VECTOR('',#15387,8.8);
#4058=VECTOR('',#15390,9.6);
#4059=VECTOR('',#15405,9.6);
#4060=VECTOR('',#15422,9.6);
#4061=VECTOR('',#15429,9.6);
#4062=VECTOR('',#15436,8.71875);
#4063=VECTOR('',#15439,7.8375);
#4064=VECTOR('',#15446,7.8375);
#4065=VECTOR('',#15455,8.71875);
#4066=VECTOR('',#15464,6.075);
#4067=VECTOR('',#15473,8.71875);
#4068=VECTOR('',#15478,9.6);
#4069=VECTOR('',#15485,9.6);
#4070=VECTOR('',#15488,6.075);
#4071=VECTOR('',#15493,6.075);
#4072=VECTOR('',#15514,4.);
#4073=VECTOR('',#15533,6.075);
#4074=VECTOR('',#15536,6.075);
#4075=CIRCLE('',#11162,2.);
#4076=CIRCLE('',#11163,2.);
#4077=CIRCLE('',#11165,2.);
#4078=CIRCLE('',#11166,2.);
#4079=CIRCLE('',#11168,4.);
#4080=CIRCLE('',#11169,4.);
#4081=CIRCLE('',#11171,2.25000000000001);
#4082=CIRCLE('',#11172,2.25);
#4083=CIRCLE('',#11174,4.);
#4084=CIRCLE('',#11175,4.);
#4085=CIRCLE('',#11177,2.25000000000001);
#4086=CIRCLE('',#11178,2.25);
#4087=CIRCLE('',#11180,7.00000000000001);
#4088=CIRCLE('',#11181,7.00000000000001);
#4089=CIRCLE('',#11183,10.);
#4090=CIRCLE('',#11184,10.);
#4091=CIRCLE('',#11186,11.1);
#4092=CIRCLE('',#11187,11.1);
#4093=CIRCLE('',#11190,2.);
#4094=CIRCLE('',#11192,2.);
#4095=CIRCLE('',#11194,12.5);
#4096=CIRCLE('',#11197,12.5);
#4097=CIRCLE('',#11202,2.);
#4098=CIRCLE('',#11203,2.);
#4099=CIRCLE('',#11235,2.);
#4100=CIRCLE('',#11236,2.);
#4101=CIRCLE('',#11238,2.);
#4102=CIRCLE('',#11239,2.);
#4103=CIRCLE('',#11241,4.);
#4104=CIRCLE('',#11242,4.);
#4105=CIRCLE('',#11244,2.25000000000001);
#4106=CIRCLE('',#11245,2.25);
#4107=CIRCLE('',#11247,4.);
#4108=CIRCLE('',#11248,4.);
#4109=CIRCLE('',#11250,2.25000000000001);
#4110=CIRCLE('',#11251,2.25);
#4111=CIRCLE('',#11253,7.00000000000001);
#4112=CIRCLE('',#11254,7.00000000000001);
#4113=CIRCLE('',#11256,10.);
#4114=CIRCLE('',#11257,10.);
#4115=CIRCLE('',#11259,11.1);
#4116=CIRCLE('',#11260,11.1);
#4117=CIRCLE('',#11263,2.);
#4118=CIRCLE('',#11265,2.);
#4119=CIRCLE('',#11267,12.5);
#4120=CIRCLE('',#11270,12.5);
#4121=CIRCLE('',#11275,2.);
#4122=CIRCLE('',#11276,2.);
#4123=CIRCLE('',#11308,4.);
#4124=CIRCLE('',#11310,4.);
#4125=CIRCLE('',#11313,2.25);
#4126=CIRCLE('',#11314,2.25);
#4127=CIRCLE('',#11316,4.);
#4128=CIRCLE('',#11317,4.);
#4129=CIRCLE('',#11319,2.25);
#4130=CIRCLE('',#11320,2.25);
#4131=CIRCLE('',#11322,7.00000000000001);
#4132=CIRCLE('',#11323,7.00000000000001);
#4133=CIRCLE('',#11325,10.);
#4134=CIRCLE('',#11326,10.);
#4135=CIRCLE('',#11328,11.1);
#4136=CIRCLE('',#11329,11.1);
#4137=CIRCLE('',#11331,2.);
#4138=CIRCLE('',#11333,2.);
#4139=CIRCLE('',#11337,12.5);
#4140=CIRCLE('',#11338,12.5);
#4141=CIRCLE('',#11341,4.);
#4142=CIRCLE('',#11342,4.);
#4143=CIRCLE('',#11345,2.);
#4144=CIRCLE('',#11346,2.);
#4145=CIRCLE('',#11356,4.);
#4146=CIRCLE('',#11357,4.);
#4147=CIRCLE('',#11368,4.);
#4148=CIRCLE('',#11370,4.);
#4149=CIRCLE('',#11373,2.25);
#4150=CIRCLE('',#11374,2.25);
#4151=CIRCLE('',#11376,4.);
#4152=CIRCLE('',#11377,4.);
#4153=CIRCLE('',#11379,2.25);
#4154=CIRCLE('',#11380,2.25);
#4155=CIRCLE('',#11382,7.00000000000001);
#4156=CIRCLE('',#11383,7.00000000000001);
#4157=CIRCLE('',#11385,10.);
#4158=CIRCLE('',#11386,10.);
#4159=CIRCLE('',#11388,11.1);
#4160=CIRCLE('',#11389,11.1);
#4161=CIRCLE('',#11391,2.);
#4162=CIRCLE('',#11393,2.);
#4163=CIRCLE('',#11397,12.5);
#4164=CIRCLE('',#11398,12.5);
#4165=CIRCLE('',#11401,4.);
#4166=CIRCLE('',#11402,4.);
#4167=CIRCLE('',#11405,2.);
#4168=CIRCLE('',#11406,2.);
#4169=CIRCLE('',#11416,4.);
#4170=CIRCLE('',#11417,4.);
#4171=CIRCLE('',#11428,3.);
#4172=CIRCLE('',#11429,3.);
#4173=CIRCLE('',#11431,3.);
#4174=CIRCLE('',#11432,3.);
#4175=CIRCLE('',#11434,3.25);
#4176=CIRCLE('',#11435,3.25);
#4177=CIRCLE('',#11437,3.25);
#4178=CIRCLE('',#11438,3.25);
#4179=CIRCLE('',#11440,2.25);
#4180=CIRCLE('',#11441,2.25);
#4181=CIRCLE('',#11443,1.75);
#4182=CIRCLE('',#11444,1.75);
#4183=CIRCLE('',#11446,1.75);
#4184=CIRCLE('',#11447,1.75);
#4185=CIRCLE('',#11449,3.);
#4186=CIRCLE('',#11450,3.);
#4187=CIRCLE('',#11452,1.5);
#4188=CIRCLE('',#11453,1.5);
#4189=CIRCLE('',#11455,1.5);
#4190=CIRCLE('',#11456,1.5);
#4191=CIRCLE('',#11461,4.);
#4192=CIRCLE('',#11462,4.);
#4193=CIRCLE('',#11464,4.);
#4194=CIRCLE('',#11465,4.);
#4195=CIRCLE('',#11468,3.);
#4196=CIRCLE('',#11469,3.);
#4197=CIRCLE('',#11472,3.);
#4198=CIRCLE('',#11473,3.);
#4199=CIRCLE('',#11476,3.);
#4200=CIRCLE('',#11477,3.);
#4201=CIRCLE('',#11480,3.);
#4202=CIRCLE('',#11481,3.);
#4203=CIRCLE('',#11488,5.);
#4204=CIRCLE('',#11489,5.);
#4205=CIRCLE('',#11491,5.);
#4206=CIRCLE('',#11492,5.);
#4207=CIRCLE('',#11494,5.);
#4208=CIRCLE('',#11495,5.);
#4209=CIRCLE('',#11497,5.);
#4210=CIRCLE('',#11498,5.);
#4211=CIRCLE('',#11500,5.);
#4212=CIRCLE('',#11501,5.);
#4213=CIRCLE('',#11503,5.);
#4214=CIRCLE('',#11504,5.);
#4215=CIRCLE('',#11513,7.);
#4216=CIRCLE('',#11514,0.5);
#4217=CIRCLE('',#11515,6.5);
#4218=CIRCLE('',#11517,7.);
#4219=CIRCLE('',#11518,7.);
#4220=CIRCLE('',#11519,0.5);
#4221=CIRCLE('',#11520,6.5);
#4222=CIRCLE('',#11522,7.);
#4223=CIRCLE('',#11523,0.5);
#4224=CIRCLE('',#11524,6.5);
#4225=CIRCLE('',#11526,7.);
#4226=CIRCLE('',#11527,7.);
#4227=CIRCLE('',#11528,0.5);
#4228=CIRCLE('',#11529,6.5);
#4229=CIRCLE('',#11532,5.);
#4230=CIRCLE('',#11533,5.);
#4231=CIRCLE('',#11538,2.7);
#4232=CIRCLE('',#11539,2.7);
#4233=CIRCLE('',#11541,2.7);
#4234=CIRCLE('',#11542,2.7);
#4235=CIRCLE('',#11549,4.);
#4236=CIRCLE('',#11550,4.);
#4237=CIRCLE('',#11552,12.);
#4238=CIRCLE('',#11553,0.5);
#4239=CIRCLE('',#11554,11.5);
#4240=CIRCLE('',#11556,12.);
#4241=CIRCLE('',#11557,12.);
#4242=CIRCLE('',#11558,0.5);
#4243=CIRCLE('',#11559,11.5);
#4244=CIRCLE('',#11561,12.);
#4245=CIRCLE('',#11562,0.5);
#4246=CIRCLE('',#11563,11.5);
#4247=CIRCLE('',#11565,12.);
#4248=CIRCLE('',#11566,12.);
#4249=CIRCLE('',#11567,0.5);
#4250=CIRCLE('',#11568,11.5);
#4251=CIRCLE('',#11571,10.);
#4252=CIRCLE('',#11572,10.);
#4253=CIRCLE('',#11580,1.8);
#4254=CIRCLE('',#11581,0.2);
#4255=CIRCLE('',#11582,2.);
#4256=CIRCLE('',#11583,2.);
#4257=CIRCLE('',#11585,2.);
#4258=CIRCLE('',#11587,1.);
#4259=CIRCLE('',#11588,1.);
#4260=CIRCLE('',#11590,1.);
#4261=CIRCLE('',#11591,1.);
#4262=CIRCLE('',#11593,1.5);
#4263=CIRCLE('',#11594,1.5);
#4264=CIRCLE('',#11596,1.5);
#4265=CIRCLE('',#11597,1.5);
#4266=CIRCLE('',#11599,1.);
#4267=CIRCLE('',#11600,1.);
#4268=CIRCLE('',#11602,2.75);
#4269=CIRCLE('',#11603,2.75);
#4270=CIRCLE('',#11604,2.75);
#4271=CIRCLE('',#11605,2.75);
#4272=CIRCLE('',#11606,2.75);
#4273=CIRCLE('',#11607,2.75);
#4274=CIRCLE('',#11609,10.2500000000004);
#4275=CIRCLE('',#11610,8.75000000000038);
#4276=CIRCLE('',#11612,10.2500000000004);
#4277=CIRCLE('',#11613,10.2500000000004);
#4278=CIRCLE('',#11615,11.25);
#4279=CIRCLE('',#11616,11.25);
#4280=CIRCLE('',#11617,11.25);
#4281=CIRCLE('',#11619,2.75);
#4282=CIRCLE('',#11620,2.75);
#4283=CIRCLE('',#11621,2.75);
#4284=CIRCLE('',#11622,2.75);
#4285=CIRCLE('',#11623,2.75);
#4286=CIRCLE('',#11624,2.75);
#4287=CIRCLE('',#11626,3.);
#4288=CIRCLE('',#11627,3.);
#4289=CIRCLE('',#11631,11.25);
#4290=CIRCLE('',#11632,10.2500000000004);
#4291=CIRCLE('',#11634,11.25);
#4292=CIRCLE('',#11635,11.25);
#4293=CIRCLE('',#11641,3.);
#4294=CIRCLE('',#11643,3.);
#4295=CIRCLE('',#11651,8.75000000000038);
#4296=CIRCLE('',#11672,5.);
#4297=CIRCLE('',#11673,5.);
#4298=CIRCLE('',#11675,6.);
#4299=CIRCLE('',#11676,6.);
#4300=CIRCLE('',#11678,11.);
#4301=CIRCLE('',#11679,10.);
#4302=CIRCLE('',#11681,11.);
#4303=CIRCLE('',#11682,10.);
#4304=CIRCLE('',#11691,12.7);
#4305=CIRCLE('',#11692,12.7);
#4306=CIRCLE('',#11694,14.7);
#4307=CIRCLE('',#11695,14.7);
#4308=CIRCLE('',#11697,14.7);
#4309=CIRCLE('',#11698,12.7);
#4310=CIRCLE('',#11700,14.7);
#4311=CIRCLE('',#11701,12.7);
#4312=CIRCLE('',#11714,3.65);
#4313=CIRCLE('',#11715,3.65);
#4314=CIRCLE('',#11717,0.200000403400263);
#4315=CIRCLE('',#11718,0.600000196920858);
#4316=CIRCLE('',#11719,0.200000373597978);
#4317=CIRCLE('',#11720,0.199999419924102);
#4318=CIRCLE('',#11721,0.20000038104856);
#4319=CIRCLE('',#11722,1.99999965375783);
#4320=CIRCLE('',#11723,0.200000284191204);
#4321=CIRCLE('',#11724,0.200000284191204);
#4322=CIRCLE('',#11725,0.200000284191218);
#4323=CIRCLE('',#11726,0.60000037573478);
#4324=CIRCLE('',#11727,0.200000284191204);
#4325=CIRCLE('',#11728,0.20000028419119);
#4326=CIRCLE('',#11729,0.60000037573478);
#4327=CIRCLE('',#11730,0.200000284191218);
#4328=CIRCLE('',#11731,0.200000284191204);
#4329=CIRCLE('',#11732,0.200000284191218);
#4330=CIRCLE('',#11733,1.99999965375781);
#4331=CIRCLE('',#11734,0.200000381048546);
#4332=CIRCLE('',#11735,0.199999419924102);
#4333=CIRCLE('',#11736,0.200000373597978);
#4334=CIRCLE('',#11737,0.600000196920858);
#4335=CIRCLE('',#11738,0.200000403400263);
#4336=CIRCLE('',#11739,0.200000403400263);
#4337=CIRCLE('',#11740,0.600000196920858);
#4338=CIRCLE('',#11741,0.200000373597978);
#4339=CIRCLE('',#11742,0.199999419924102);
#4340=CIRCLE('',#11743,0.200000381048546);
#4341=CIRCLE('',#11744,1.99999965375781);
#4342=CIRCLE('',#11745,0.200000284191204);
#4343=CIRCLE('',#11746,0.200000284191204);
#4344=CIRCLE('',#11747,0.200000284191218);
#4345=CIRCLE('',#11748,0.600000375734794);
#4346=CIRCLE('',#11749,0.200000284191204);
#4347=CIRCLE('',#11750,0.200000284191204);
#4348=CIRCLE('',#11751,0.60000037573478);
#4349=CIRCLE('',#11752,0.200000284191218);
#4350=CIRCLE('',#11753,0.20000028419119);
#4351=CIRCLE('',#11754,0.200000284191218);
#4352=CIRCLE('',#11755,1.9999996537578);
#4353=CIRCLE('',#11756,0.200000381048532);
#4354=CIRCLE('',#11757,0.199999419924102);
#4355=CIRCLE('',#11758,0.200000373597992);
#4356=CIRCLE('',#11759,0.600000196920844);
#4357=CIRCLE('',#11760,0.200000403400263);
#4358=CIRCLE('',#11761,0.999999990441758);
#4359=CIRCLE('',#11762,0.999999990441758);
#4360=CIRCLE('',#11763,0.999999990441772);
#4361=CIRCLE('',#11764,0.999999990441772);
#4362=CIRCLE('',#11765,3.65);
#4363=CIRCLE('',#11766,5.50000000000001);
#4364=CIRCLE('',#11767,3.65);
#4365=CIRCLE('',#11768,5.50000000000001);
#4366=CIRCLE('',#11769,3.65);
#4367=CIRCLE('',#11770,5.50000000000001);
#4368=CIRCLE('',#11771,5.50000000000001);
#4369=CIRCLE('',#11772,0.999999990441758);
#4370=CIRCLE('',#11773,0.999999990441758);
#4371=CIRCLE('',#11774,0.999999990441758);
#4372=CIRCLE('',#11775,0.999999990441758);
#4373=CIRCLE('',#11776,0.999999990441758);
#4374=CIRCLE('',#11777,0.999999990441772);
#4375=CIRCLE('',#11778,0.999999990441772);
#4376=CIRCLE('',#11779,0.999999990441758);
#4377=CIRCLE('',#11780,0.999999990441758);
#4378=CIRCLE('',#11781,0.999999990441758);
#4379=CIRCLE('',#11782,0.999999990441758);
#4380=CIRCLE('',#11783,0.999999990441758);
#4381=CIRCLE('',#11785,0.200000403400263);
#4382=CIRCLE('',#11786,0.600000196920844);
#4383=CIRCLE('',#11787,0.200000373597992);
#4384=CIRCLE('',#11788,0.199999419924102);
#4385=CIRCLE('',#11789,0.200000381048532);
#4386=CIRCLE('',#11790,1.9999996537578);
#4387=CIRCLE('',#11791,0.200000284191218);
#4388=CIRCLE('',#11792,0.20000028419119);
#4389=CIRCLE('',#11793,0.200000284191218);
#4390=CIRCLE('',#11794,0.60000037573478);
#4391=CIRCLE('',#11795,0.200000284191204);
#4392=CIRCLE('',#11796,0.200000284191204);
#4393=CIRCLE('',#11797,0.600000375734794);
#4394=CIRCLE('',#11798,0.200000284191218);
#4395=CIRCLE('',#11799,0.200000284191204);
#4396=CIRCLE('',#11800,0.200000284191204);
#4397=CIRCLE('',#11801,1.99999965375781);
#4398=CIRCLE('',#11802,0.200000381048546);
#4399=CIRCLE('',#11803,0.199999419924102);
#4400=CIRCLE('',#11804,0.200000373597978);
#4401=CIRCLE('',#11805,0.600000196920858);
#4402=CIRCLE('',#11806,0.200000403400263);
#4403=CIRCLE('',#11807,0.200000403400263);
#4404=CIRCLE('',#11808,0.600000196920858);
#4405=CIRCLE('',#11809,0.200000373597978);
#4406=CIRCLE('',#11810,0.199999419924102);
#4407=CIRCLE('',#11811,0.200000381048546);
#4408=CIRCLE('',#11812,1.99999965375781);
#4409=CIRCLE('',#11813,0.200000284191218);
#4410=CIRCLE('',#11814,0.200000284191204);
#4411=CIRCLE('',#11815,0.200000284191218);
#4412=CIRCLE('',#11816,0.60000037573478);
#4413=CIRCLE('',#11817,0.20000028419119);
#4414=CIRCLE('',#11818,0.200000284191204);
#4415=CIRCLE('',#11819,0.60000037573478);
#4416=CIRCLE('',#11820,0.200000284191218);
#4417=CIRCLE('',#11821,0.200000284191204);
#4418=CIRCLE('',#11822,0.200000284191204);
#4419=CIRCLE('',#11823,1.99999965375783);
#4420=CIRCLE('',#11824,0.20000038104856);
#4421=CIRCLE('',#11825,0.199999419924102);
#4422=CIRCLE('',#11826,0.200000373597978);
#4423=CIRCLE('',#11827,0.600000196920858);
#4424=CIRCLE('',#11828,0.200000403400263);
#4425=CIRCLE('',#11829,0.999999990441758);
#4426=CIRCLE('',#11830,0.999999990441772);
#4427=CIRCLE('',#11831,0.999999990441772);
#4428=CIRCLE('',#11832,0.999999990441758);
#4429=CIRCLE('',#11833,0.999999990441758);
#4430=CIRCLE('',#11834,0.999999990441758);
#4431=CIRCLE('',#11835,0.999999990441758);
#4432=CIRCLE('',#11836,0.999999990441758);
#4433=CIRCLE('',#11837,0.999999990441758);
#4434=CIRCLE('',#11838,0.999999990441758);
#4435=CIRCLE('',#11839,0.999999990441758);
#4436=CIRCLE('',#11840,0.999999990441758);
#4437=CIRCLE('',#11841,0.999999990441758);
#4438=CIRCLE('',#11842,0.999999990441758);
#4439=CIRCLE('',#11843,0.999999990441772);
#4440=CIRCLE('',#11844,0.999999990441772);
#4441=CIRCLE('',#11845,3.65);
#4442=CIRCLE('',#11846,5.50000000000001);
#4443=CIRCLE('',#11847,5.50000000000001);
#4444=CIRCLE('',#11848,3.65);
#4445=CIRCLE('',#11849,5.50000000000001);
#4446=CIRCLE('',#11850,3.65);
#4447=CIRCLE('',#11851,5.50000000000001);
#4448=CIRCLE('',#12017,2.25);
#4449=CIRCLE('',#12018,2.25);
#4450=CIRCLE('',#12020,2.25);
#4451=CIRCLE('',#12021,2.25);
#4452=CIRCLE('',#12023,5.);
#4453=CIRCLE('',#12025,5.);
#4454=CIRCLE('',#12027,5.);
#4455=CIRCLE('',#12030,5.);
#4456=CIRCLE('',#12031,5.);
#4457=CIRCLE('',#12034,5.);
#4458=CIRCLE('',#12037,5.);
#4459=CIRCLE('',#12038,5.);
#4460=CIRCLE('',#12041,2.);
#4461=CIRCLE('',#12042,2.);
#4462=CIRCLE('',#12043,2.);
#4463=CIRCLE('',#12044,2.);
#4464=CIRCLE('',#12045,4.);
#4465=CIRCLE('',#12046,4.);
#4466=CIRCLE('',#12048,2.);
#4467=CIRCLE('',#12049,2.);
#4468=CIRCLE('',#12050,2.);
#4469=CIRCLE('',#12051,2.);
#4470=CIRCLE('',#12052,4.);
#4471=CIRCLE('',#12053,4.);
#4472=CIRCLE('',#12065,2.);
#4473=CIRCLE('',#12066,2.);
#4474=CIRCLE('',#12068,2.);
#4475=CIRCLE('',#12069,2.);
#4476=CIRCLE('',#12072,2.);
#4477=CIRCLE('',#12073,2.);
#4478=CIRCLE('',#12075,2.);
#4479=CIRCLE('',#12076,2.);
#4480=CIRCLE('',#12086,4.);
#4481=CIRCLE('',#12087,3.99999999999999);
#4482=CIRCLE('',#12089,2.15);
#4483=CIRCLE('',#12090,2.15);
#4484=CIRCLE('',#12092,4.);
#4485=CIRCLE('',#12093,4.);
#4486=CIRCLE('',#12101,4.);
#4487=CIRCLE('',#12102,4.);
#4488=CIRCLE('',#12114,4.);
#4489=CIRCLE('',#12115,4.);
#4490=CIRCLE('',#12116,4.);
#4491=CIRCLE('',#12117,4.);
#4492=CIRCLE('',#12119,4.);
#4493=CIRCLE('',#12120,4.);
#4494=CIRCLE('',#12121,4.);
#4495=CIRCLE('',#12122,4.);
#4496=CIRCLE('',#12137,9.);
#4497=CIRCLE('',#12138,9.);
#4498=CIRCLE('',#12140,12.7);
#4499=CIRCLE('',#12141,12.7);
#4500=CIRCLE('',#12142,12.);
#4501=CIRCLE('',#12144,12.);
#4502=CIRCLE('',#12146,6.2);
#4503=CIRCLE('',#12147,6.2);
#4504=CIRCLE('',#12149,6.2);
#4505=CIRCLE('',#12150,6.2);
#4506=CIRCLE('',#12152,4.2);
#4507=CIRCLE('',#12153,4.2);
#4508=CIRCLE('',#12155,4.2);
#4509=CIRCLE('',#12156,4.2);
#4510=CIRCLE('',#12165,1.9845);
#4511=CIRCLE('',#12167,1.9845);
#4512=CIRCLE('',#12169,1.9845);
#4513=CIRCLE('',#12171,1.9845);
#4514=CIRCLE('',#12173,1.9845);
#4515=CIRCLE('',#12175,1.9845);
#4516=CIRCLE('',#12177,1.9845);
#4517=CIRCLE('',#12179,11.);
#4518=CIRCLE('',#12180,0.3);
#4519=CIRCLE('',#12181,10.7);
#4520=CIRCLE('',#12183,11.);
#4521=CIRCLE('',#12185,10.7);
#4522=CIRCLE('',#12186,0.3);
#4523=CIRCLE('',#12188,9.6);
#4524=CIRCLE('',#12189,9.6);
#4525=CIRCLE('',#12191,9.6);
#4526=CIRCLE('',#12192,0.18);
#4527=CIRCLE('',#12194,8.8);
#4528=CIRCLE('',#12196,8.8);
#4529=CIRCLE('',#12198,8.8);
#4530=CIRCLE('',#12199,1.9845);
#4531=CIRCLE('',#12201,8.8);
#4532=CIRCLE('',#12202,8.8);
#4533=CIRCLE('',#12204,9.6);
#4534=CIRCLE('',#12205,9.6);
#4535=CIRCLE('',#12207,9.6);
#4536=CIRCLE('',#12208,0.18);
#4537=CIRCLE('',#12210,9.6);
#4538=CIRCLE('',#12214,6.075);
#4539=CIRCLE('',#12215,1.9845);
#4540=CIRCLE('',#12216,6.075);
#4541=CIRCLE('',#12218,9.6);
#4542=CIRCLE('',#12219,8.71875);
#4543=CIRCLE('',#12221,9.6);
#4544=CIRCLE('',#12223,8.71875);
#4545=CIRCLE('',#12224,8.71875);
#4546=CIRCLE('',#12226,7.8375);
#4547=CIRCLE('',#12228,6.075);
#4548=CIRCLE('',#12229,7.8375);
#4549=CIRCLE('',#12230,6.075);
#4550=CIRCLE('',#12232,9.6);
#4551=CIRCLE('',#12233,8.71875);
#4552=CIRCLE('',#12234,9.6);
#4553=CIRCLE('',#12236,6.075);
#4554=CIRCLE('',#12237,7.8375);
#4555=CIRCLE('',#12239,8.71875);
#4556=CIRCLE('',#12240,8.71875);
#4557=CIRCLE('',#12241,7.8375);
#4558=CIRCLE('',#12243,9.6);
#4559=CIRCLE('',#12244,9.6);
#4560=CIRCLE('',#12248,6.075);
#4561=CIRCLE('',#12249,6.075);
#4562=CIRCLE('',#12251,5.975);
#4563=CIRCLE('',#12252,0.1);
#4564=CIRCLE('',#12254,4.);
#4565=CIRCLE('',#12255,0.3);
#4566=CIRCLE('',#12256,4.3);
#4567=CIRCLE('',#12258,4.);
#4568=CIRCLE('',#12260,4.3);
#4569=CIRCLE('',#12261,0.3);
#4570=CIRCLE('',#12263,6.075);
#4571=CIRCLE('',#12264,0.1);
#4572=CIRCLE('',#12265,5.975);
#4573=CIRCLE('',#12267,6.075);
#4574=VERTEX_POINT('',#15608);
#4575=VERTEX_POINT('',#15610);
#4576=VERTEX_POINT('',#15614);
#4577=VERTEX_POINT('',#15616);
#4578=VERTEX_POINT('',#15620);
#4579=VERTEX_POINT('',#15622);
#4580=VERTEX_POINT('',#15626);
#4581=VERTEX_POINT('',#15628);
#4582=VERTEX_POINT('',#15632);
#4583=VERTEX_POINT('',#15634);
#4584=VERTEX_POINT('',#15638);
#4585=VERTEX_POINT('',#15640);
#4586=VERTEX_POINT('',#15644);
#4587=VERTEX_POINT('',#15646);
#4588=VERTEX_POINT('',#15650);
#4589=VERTEX_POINT('',#15652);
#4590=VERTEX_POINT('',#15656);
#4591=VERTEX_POINT('',#15658);
#4592=VERTEX_POINT('',#15662);
#4593=VERTEX_POINT('',#15663);
#4594=VERTEX_POINT('',#15665);
#4595=VERTEX_POINT('',#15667);
#4596=VERTEX_POINT('',#15669);
#4597=VERTEX_POINT('',#15671);
#4598=VERTEX_POINT('',#15673);
#4599=VERTEX_POINT('',#15675);
#4600=VERTEX_POINT('',#15677);
#4601=VERTEX_POINT('',#15679);
#4602=VERTEX_POINT('',#15683);
#4603=VERTEX_POINT('',#15685);
#4604=VERTEX_POINT('',#15687);
#4605=VERTEX_POINT('',#15691);
#4606=VERTEX_POINT('',#15693);
#4607=VERTEX_POINT('',#15695);
#4608=VERTEX_POINT('',#15699);
#4609=VERTEX_POINT('',#15700);
#4610=VERTEX_POINT('',#15702);
#4611=VERTEX_POINT('',#15704);
#4612=VERTEX_POINT('',#15706);
#4613=VERTEX_POINT('',#15708);
#4614=VERTEX_POINT('',#15711);
#4615=VERTEX_POINT('',#15714);
#4616=VERTEX_POINT('',#15715);
#4617=VERTEX_POINT('',#15717);
#4618=VERTEX_POINT('',#15719);
#4619=VERTEX_POINT('',#15721);
#4620=VERTEX_POINT('',#15723);
#4621=VERTEX_POINT('',#15726);
#4622=VERTEX_POINT('',#15727);
#4623=VERTEX_POINT('',#15729);
#4624=VERTEX_POINT('',#15731);
#4625=VERTEX_POINT('',#15733);
#4626=VERTEX_POINT('',#15735);
#4627=VERTEX_POINT('',#15739);
#4628=VERTEX_POINT('',#15741);
#4629=VERTEX_POINT('',#15745);
#4630=VERTEX_POINT('',#15749);
#4631=VERTEX_POINT('',#15752);
#4632=VERTEX_POINT('',#15756);
#4633=VERTEX_POINT('',#15758);
#4634=VERTEX_POINT('',#15760);
#4635=VERTEX_POINT('',#15763);
#4636=VERTEX_POINT('',#15767);
#4637=VERTEX_POINT('',#15776);
#4638=VERTEX_POINT('',#15780);
#4639=VERTEX_POINT('',#15784);
#4640=VERTEX_POINT('',#15786);
#4641=VERTEX_POINT('',#15794);
#4642=VERTEX_POINT('',#15796);
#4643=VERTEX_POINT('',#15800);
#4644=VERTEX_POINT('',#15804);
#4645=VERTEX_POINT('',#15808);
#4646=VERTEX_POINT('',#15812);
#4647=VERTEX_POINT('',#15819);
#4648=VERTEX_POINT('',#15821);
#4649=VERTEX_POINT('',#15825);
#4650=VERTEX_POINT('',#15829);
#4651=VERTEX_POINT('',#15833);
#4652=VERTEX_POINT('',#15837);
#4653=VERTEX_POINT('',#15855);
#4654=VERTEX_POINT('',#15857);
#4655=VERTEX_POINT('',#15861);
#4656=VERTEX_POINT('',#15863);
#4657=VERTEX_POINT('',#15867);
#4658=VERTEX_POINT('',#15869);
#4659=VERTEX_POINT('',#15873);
#4660=VERTEX_POINT('',#15875);
#4661=VERTEX_POINT('',#15879);
#4662=VERTEX_POINT('',#15881);
#4663=VERTEX_POINT('',#15885);
#4664=VERTEX_POINT('',#15887);
#4665=VERTEX_POINT('',#15891);
#4666=VERTEX_POINT('',#15893);
#4667=VERTEX_POINT('',#15897);
#4668=VERTEX_POINT('',#15899);
#4669=VERTEX_POINT('',#15903);
#4670=VERTEX_POINT('',#15905);
#4671=VERTEX_POINT('',#15909);
#4672=VERTEX_POINT('',#15910);
#4673=VERTEX_POINT('',#15912);
#4674=VERTEX_POINT('',#15914);
#4675=VERTEX_POINT('',#15916);
#4676=VERTEX_POINT('',#15918);
#4677=VERTEX_POINT('',#15920);
#4678=VERTEX_POINT('',#15922);
#4679=VERTEX_POINT('',#15924);
#4680=VERTEX_POINT('',#15926);
#4681=VERTEX_POINT('',#15930);
#4682=VERTEX_POINT('',#15932);
#4683=VERTEX_POINT('',#15934);
#4684=VERTEX_POINT('',#15938);
#4685=VERTEX_POINT('',#15940);
#4686=VERTEX_POINT('',#15942);
#4687=VERTEX_POINT('',#15946);
#4688=VERTEX_POINT('',#15947);
#4689=VERTEX_POINT('',#15949);
#4690=VERTEX_POINT('',#15952);
#4691=VERTEX_POINT('',#15954);
#4692=VERTEX_POINT('',#15956);
#4693=VERTEX_POINT('',#15958);
#4694=VERTEX_POINT('',#15961);
#4695=VERTEX_POINT('',#15962);
#4696=VERTEX_POINT('',#15964);
#4697=VERTEX_POINT('',#15966);
#4698=VERTEX_POINT('',#15968);
#4699=VERTEX_POINT('',#15970);
#4700=VERTEX_POINT('',#15973);
#4701=VERTEX_POINT('',#15974);
#4702=VERTEX_POINT('',#15976);
#4703=VERTEX_POINT('',#15978);
#4704=VERTEX_POINT('',#15980);
#4705=VERTEX_POINT('',#15982);
#4706=VERTEX_POINT('',#15986);
#4707=VERTEX_POINT('',#15988);
#4708=VERTEX_POINT('',#15992);
#4709=VERTEX_POINT('',#15996);
#4710=VERTEX_POINT('',#15999);
#4711=VERTEX_POINT('',#16003);
#4712=VERTEX_POINT('',#16005);
#4713=VERTEX_POINT('',#16008);
#4714=VERTEX_POINT('',#16010);
#4715=VERTEX_POINT('',#16014);
#4716=VERTEX_POINT('',#16023);
#4717=VERTEX_POINT('',#16027);
#4718=VERTEX_POINT('',#16031);
#4719=VERTEX_POINT('',#16033);
#4720=VERTEX_POINT('',#16041);
#4721=VERTEX_POINT('',#16043);
#4722=VERTEX_POINT('',#16047);
#4723=VERTEX_POINT('',#16051);
#4724=VERTEX_POINT('',#16055);
#4725=VERTEX_POINT('',#16059);
#4726=VERTEX_POINT('',#16066);
#4727=VERTEX_POINT('',#16068);
#4728=VERTEX_POINT('',#16072);
#4729=VERTEX_POINT('',#16076);
#4730=VERTEX_POINT('',#16080);
#4731=VERTEX_POINT('',#16084);
#4732=VERTEX_POINT('',#16102);
#4733=VERTEX_POINT('',#16104);
#4734=VERTEX_POINT('',#16106);
#4735=VERTEX_POINT('',#16108);
#4736=VERTEX_POINT('',#16112);
#4737=VERTEX_POINT('',#16114);
#4738=VERTEX_POINT('',#16118);
#4739=VERTEX_POINT('',#16120);
#4740=VERTEX_POINT('',#16124);
#4741=VERTEX_POINT('',#16126);
#4742=VERTEX_POINT('',#16130);
#4743=VERTEX_POINT('',#16132);
#4744=VERTEX_POINT('',#16136);
#4745=VERTEX_POINT('',#16138);
#4746=VERTEX_POINT('',#16142);
#4747=VERTEX_POINT('',#16144);
#4748=VERTEX_POINT('',#16148);
#4749=VERTEX_POINT('',#16149);
#4750=VERTEX_POINT('',#16151);
#4751=VERTEX_POINT('',#16153);
#4752=VERTEX_POINT('',#16155);
#4753=VERTEX_POINT('',#16159);
#4754=VERTEX_POINT('',#16160);
#4755=VERTEX_POINT('',#16162);
#4756=VERTEX_POINT('',#16164);
#4757=VERTEX_POINT('',#16166);
#4758=VERTEX_POINT('',#16170);
#4759=VERTEX_POINT('',#16172);
#4760=VERTEX_POINT('',#16175);
#4761=VERTEX_POINT('',#16177);
#4762=VERTEX_POINT('',#16181);
#4763=VERTEX_POINT('',#16183);
#4764=VERTEX_POINT('',#16185);
#4765=VERTEX_POINT('',#16189);
#4766=VERTEX_POINT('',#16191);
#4767=VERTEX_POINT('',#16196);
#4768=VERTEX_POINT('',#16200);
#4769=VERTEX_POINT('',#16202);
#4770=VERTEX_POINT('',#16204);
#4771=VERTEX_POINT('',#16206);
#4772=VERTEX_POINT('',#16208);
#4773=VERTEX_POINT('',#16210);
#4774=VERTEX_POINT('',#16212);
#4775=VERTEX_POINT('',#16214);
#4776=VERTEX_POINT('',#16217);
#4777=VERTEX_POINT('',#16219);
#4778=VERTEX_POINT('',#16223);
#4779=VERTEX_POINT('',#16227);
#4780=VERTEX_POINT('',#16231);
#4781=VERTEX_POINT('',#16243);
#4782=VERTEX_POINT('',#16244);
#4783=VERTEX_POINT('',#16249);
#4784=VERTEX_POINT('',#16251);
#4785=VERTEX_POINT('',#16253);
#4786=VERTEX_POINT('',#16255);
#4787=VERTEX_POINT('',#16274);
#4788=VERTEX_POINT('',#16276);
#4789=VERTEX_POINT('',#16278);
#4790=VERTEX_POINT('',#16280);
#4791=VERTEX_POINT('',#16284);
#4792=VERTEX_POINT('',#16286);
#4793=VERTEX_POINT('',#16290);
#4794=VERTEX_POINT('',#16292);
#4795=VERTEX_POINT('',#16296);
#4796=VERTEX_POINT('',#16298);
#4797=VERTEX_POINT('',#16302);
#4798=VERTEX_POINT('',#16304);
#4799=VERTEX_POINT('',#16308);
#4800=VERTEX_POINT('',#16310);
#4801=VERTEX_POINT('',#16314);
#4802=VERTEX_POINT('',#16316);
#4803=VERTEX_POINT('',#16320);
#4804=VERTEX_POINT('',#16321);
#4805=VERTEX_POINT('',#16323);
#4806=VERTEX_POINT('',#16325);
#4807=VERTEX_POINT('',#16327);
#4808=VERTEX_POINT('',#16331);
#4809=VERTEX_POINT('',#16332);
#4810=VERTEX_POINT('',#16334);
#4811=VERTEX_POINT('',#16336);
#4812=VERTEX_POINT('',#16338);
#4813=VERTEX_POINT('',#16342);
#4814=VERTEX_POINT('',#16344);
#4815=VERTEX_POINT('',#16346);
#4816=VERTEX_POINT('',#16349);
#4817=VERTEX_POINT('',#16353);
#4818=VERTEX_POINT('',#16355);
#4819=VERTEX_POINT('',#16357);
#4820=VERTEX_POINT('',#16361);
#4821=VERTEX_POINT('',#16363);
#4822=VERTEX_POINT('',#16367);
#4823=VERTEX_POINT('',#16372);
#4824=VERTEX_POINT('',#16374);
#4825=VERTEX_POINT('',#16376);
#4826=VERTEX_POINT('',#16379);
#4827=VERTEX_POINT('',#16381);
#4828=VERTEX_POINT('',#16383);
#4829=VERTEX_POINT('',#16385);
#4830=VERTEX_POINT('',#16387);
#4831=VERTEX_POINT('',#16389);
#4832=VERTEX_POINT('',#16391);
#4833=VERTEX_POINT('',#16395);
#4834=VERTEX_POINT('',#16399);
#4835=VERTEX_POINT('',#16402);
#4836=VERTEX_POINT('',#16415);
#4837=VERTEX_POINT('',#16416);
#4838=VERTEX_POINT('',#16421);
#4839=VERTEX_POINT('',#16423);
#4840=VERTEX_POINT('',#16425);
#4841=VERTEX_POINT('',#16427);
#4842=VERTEX_POINT('',#16446);
#4843=VERTEX_POINT('',#16448);
#4844=VERTEX_POINT('',#16452);
#4845=VERTEX_POINT('',#16454);
#4846=VERTEX_POINT('',#16458);
#4847=VERTEX_POINT('',#16460);
#4848=VERTEX_POINT('',#16464);
#4849=VERTEX_POINT('',#16466);
#4850=VERTEX_POINT('',#16470);
#4851=VERTEX_POINT('',#16472);
#4852=VERTEX_POINT('',#16476);
#4853=VERTEX_POINT('',#16478);
#4854=VERTEX_POINT('',#16482);
#4855=VERTEX_POINT('',#16484);
#4856=VERTEX_POINT('',#16488);
#4857=VERTEX_POINT('',#16490);
#4858=VERTEX_POINT('',#16494);
#4859=VERTEX_POINT('',#16496);
#4860=VERTEX_POINT('',#16500);
#4861=VERTEX_POINT('',#16502);
#4862=VERTEX_POINT('',#16506);
#4863=VERTEX_POINT('',#16507);
#4864=VERTEX_POINT('',#16509);
#4865=VERTEX_POINT('',#16511);
#4866=VERTEX_POINT('',#16515);
#4867=VERTEX_POINT('',#16516);
#4868=VERTEX_POINT('',#16518);
#4869=VERTEX_POINT('',#16520);
#4870=VERTEX_POINT('',#16524);
#4871=VERTEX_POINT('',#16525);
#4872=VERTEX_POINT('',#16527);
#4873=VERTEX_POINT('',#16529);
#4874=VERTEX_POINT('',#16539);
#4875=VERTEX_POINT('',#16540);
#4876=VERTEX_POINT('',#16542);
#4877=VERTEX_POINT('',#16544);
#4878=VERTEX_POINT('',#16548);
#4879=VERTEX_POINT('',#16550);
#4880=VERTEX_POINT('',#16554);
#4881=VERTEX_POINT('',#16556);
#4882=VERTEX_POINT('',#16560);
#4883=VERTEX_POINT('',#16562);
#4884=VERTEX_POINT('',#16566);
#4885=VERTEX_POINT('',#16568);
#4886=VERTEX_POINT('',#16572);
#4887=VERTEX_POINT('',#16574);
#4888=VERTEX_POINT('',#16578);
#4889=VERTEX_POINT('',#16580);
#4890=VERTEX_POINT('',#16587);
#4891=VERTEX_POINT('',#16588);
#4892=VERTEX_POINT('',#16590);
#4893=VERTEX_POINT('',#16592);
#4894=VERTEX_POINT('',#16596);
#4895=VERTEX_POINT('',#16597);
#4896=VERTEX_POINT('',#16599);
#4897=VERTEX_POINT('',#16601);
#4898=VERTEX_POINT('',#16605);
#4899=VERTEX_POINT('',#16606);
#4900=VERTEX_POINT('',#16608);
#4901=VERTEX_POINT('',#16610);
#4902=VERTEX_POINT('',#16614);
#4903=VERTEX_POINT('',#16615);
#4904=VERTEX_POINT('',#16617);
#4905=VERTEX_POINT('',#16619);
#4906=VERTEX_POINT('',#16623);
#4907=VERTEX_POINT('',#16624);
#4908=VERTEX_POINT('',#16626);
#4909=VERTEX_POINT('',#16628);
#4910=VERTEX_POINT('',#16657);
#4911=VERTEX_POINT('',#16659);
#4912=VERTEX_POINT('',#16663);
#4913=VERTEX_POINT('',#16664);
#4914=VERTEX_POINT('',#16667);
#4915=VERTEX_POINT('',#16671);
#4916=VERTEX_POINT('',#16673);
#4917=VERTEX_POINT('',#16677);
#4918=VERTEX_POINT('',#16678);
#4919=VERTEX_POINT('',#16681);
#4920=VERTEX_POINT('',#16687);
#4921=VERTEX_POINT('',#16689);
#4922=VERTEX_POINT('',#16697);
#4923=VERTEX_POINT('',#16698);
#4924=VERTEX_POINT('',#16700);
#4925=VERTEX_POINT('',#16702);
#4926=VERTEX_POINT('',#16706);
#4927=VERTEX_POINT('',#16707);
#4928=VERTEX_POINT('',#16709);
#4929=VERTEX_POINT('',#16711);
#4930=VERTEX_POINT('',#16724);
#4931=VERTEX_POINT('',#16726);
#4932=VERTEX_POINT('',#16730);
#4933=VERTEX_POINT('',#16732);
#4934=VERTEX_POINT('',#16736);
#4935=VERTEX_POINT('',#16737);
#4936=VERTEX_POINT('',#16740);
#4937=VERTEX_POINT('',#16744);
#4938=VERTEX_POINT('',#16746);
#4939=VERTEX_POINT('',#16750);
#4940=VERTEX_POINT('',#16751);
#4941=VERTEX_POINT('',#16754);
#4942=VERTEX_POINT('',#16760);
#4943=VERTEX_POINT('',#16762);
#4944=VERTEX_POINT('',#16773);
#4945=VERTEX_POINT('',#16775);
#4946=VERTEX_POINT('',#16777);
#4947=VERTEX_POINT('',#16781);
#4948=VERTEX_POINT('',#16785);
#4949=VERTEX_POINT('',#16787);
#4950=VERTEX_POINT('',#16791);
#4951=VERTEX_POINT('',#16793);
#4952=VERTEX_POINT('',#16797);
#4953=VERTEX_POINT('',#16799);
#4954=VERTEX_POINT('',#16803);
#4955=VERTEX_POINT('',#16805);
#4956=VERTEX_POINT('',#16809);
#4957=VERTEX_POINT('',#16811);
#4958=VERTEX_POINT('',#16815);
#4959=VERTEX_POINT('',#16817);
#4960=VERTEX_POINT('',#16819);
#4961=VERTEX_POINT('',#16821);
#4962=VERTEX_POINT('',#16823);
#4963=VERTEX_POINT('',#16825);
#4964=VERTEX_POINT('',#16827);
#4965=VERTEX_POINT('',#16829);
#4966=VERTEX_POINT('',#16831);
#4967=VERTEX_POINT('',#16833);
#4968=VERTEX_POINT('',#16837);
#4969=VERTEX_POINT('',#16838);
#4970=VERTEX_POINT('',#16840);
#4971=VERTEX_POINT('',#16855);
#4972=VERTEX_POINT('',#16872);
#4973=VERTEX_POINT('',#16873);
#4974=VERTEX_POINT('',#16875);
#4975=VERTEX_POINT('',#16877);
#4976=VERTEX_POINT('',#16881);
#4977=VERTEX_POINT('',#16882);
#4978=VERTEX_POINT('',#16884);
#4979=VERTEX_POINT('',#16886);
#4980=VERTEX_POINT('',#16888);
#4981=VERTEX_POINT('',#16892);
#4982=VERTEX_POINT('',#16894);
#4983=VERTEX_POINT('',#16896);
#4984=VERTEX_POINT('',#16898);
#4985=VERTEX_POINT('',#16900);
#4986=VERTEX_POINT('',#16902);
#4987=VERTEX_POINT('',#16904);
#4988=VERTEX_POINT('',#16906);
#4989=VERTEX_POINT('',#16908);
#4990=VERTEX_POINT('',#16910);
#4991=VERTEX_POINT('',#16914);
#4992=VERTEX_POINT('',#16916);
#4993=VERTEX_POINT('',#16918);
#4994=VERTEX_POINT('',#16920);
#4995=VERTEX_POINT('',#16922);
#4996=VERTEX_POINT('',#16924);
#4997=VERTEX_POINT('',#16926);
#4998=VERTEX_POINT('',#16928);
#4999=VERTEX_POINT('',#16932);
#5000=VERTEX_POINT('',#16933);
#5001=VERTEX_POINT('',#16937);
#5002=VERTEX_POINT('',#16938);
#5003=VERTEX_POINT('',#16940);
#5004=VERTEX_POINT('',#16942);
#5005=VERTEX_POINT('',#16949);
#5006=VERTEX_POINT('',#16952);
#5007=VERTEX_POINT('',#16954);
#5008=VERTEX_POINT('',#16958);
#5009=VERTEX_POINT('',#16960);
#5010=VERTEX_POINT('',#16966);
#5011=VERTEX_POINT('',#16968);
#5012=VERTEX_POINT('',#16975);
#5013=VERTEX_POINT('',#16981);
#5014=VERTEX_POINT('',#16996);
#5015=VERTEX_POINT('',#16997);
#5016=VERTEX_POINT('',#17048);
#5017=VERTEX_POINT('',#17050);
#5018=VERTEX_POINT('',#17054);
#5019=VERTEX_POINT('',#17058);
#5020=VERTEX_POINT('',#17067);
#5021=VERTEX_POINT('',#17068);
#5022=VERTEX_POINT('',#17070);
#5023=VERTEX_POINT('',#17072);
#5024=VERTEX_POINT('',#17076);
#5025=VERTEX_POINT('',#17077);
#5026=VERTEX_POINT('',#17079);
#5027=VERTEX_POINT('',#17081);
#5028=VERTEX_POINT('',#17085);
#5029=VERTEX_POINT('',#17087);
#5030=VERTEX_POINT('',#17090);
#5031=VERTEX_POINT('',#17092);
#5032=VERTEX_POINT('',#17096);
#5033=VERTEX_POINT('',#17098);
#5034=VERTEX_POINT('',#17101);
#5035=VERTEX_POINT('',#17103);
#5036=VERTEX_POINT('',#17118);
#5037=VERTEX_POINT('',#17119);
#5038=VERTEX_POINT('',#17121);
#5039=VERTEX_POINT('',#17123);
#5040=VERTEX_POINT('',#17127);
#5041=VERTEX_POINT('',#17128);
#5042=VERTEX_POINT('',#17130);
#5043=VERTEX_POINT('',#17132);
#5044=VERTEX_POINT('',#17136);
#5045=VERTEX_POINT('',#17138);
#5046=VERTEX_POINT('',#17140);
#5047=VERTEX_POINT('',#17142);
#5048=VERTEX_POINT('',#17145);
#5049=VERTEX_POINT('',#17147);
#5050=VERTEX_POINT('',#17149);
#5051=VERTEX_POINT('',#17151);
#5052=VERTEX_POINT('',#17155);
#5053=VERTEX_POINT('',#17157);
#5054=VERTEX_POINT('',#17159);
#5055=VERTEX_POINT('',#17161);
#5056=VERTEX_POINT('',#17164);
#5057=VERTEX_POINT('',#17166);
#5058=VERTEX_POINT('',#17168);
#5059=VERTEX_POINT('',#17170);
#5060=VERTEX_POINT('',#17193);
#5061=VERTEX_POINT('',#17194);
#5062=VERTEX_POINT('',#17196);
#5063=VERTEX_POINT('',#17198);
#5064=VERTEX_POINT('',#17202);
#5065=VERTEX_POINT('',#17203);
#5066=VERTEX_POINT('',#17205);
#5067=VERTEX_POINT('',#17207);
#5068=VERTEX_POINT('',#17209);
#5069=VERTEX_POINT('',#17211);
#5070=VERTEX_POINT('',#17213);
#5071=VERTEX_POINT('',#17215);
#5072=VERTEX_POINT('',#17217);
#5073=VERTEX_POINT('',#17219);
#5074=VERTEX_POINT('',#17221);
#5075=VERTEX_POINT('',#17223);
#5076=VERTEX_POINT('',#17225);
#5077=VERTEX_POINT('',#17227);
#5078=VERTEX_POINT('',#17229);
#5079=VERTEX_POINT('',#17231);
#5080=VERTEX_POINT('',#17233);
#5081=VERTEX_POINT('',#17235);
#5082=VERTEX_POINT('',#17237);
#5083=VERTEX_POINT('',#17239);
#5084=VERTEX_POINT('',#17241);
#5085=VERTEX_POINT('',#17243);
#5086=VERTEX_POINT('',#17245);
#5087=VERTEX_POINT('',#17247);
#5088=VERTEX_POINT('',#17249);
#5089=VERTEX_POINT('',#17251);
#5090=VERTEX_POINT('',#17253);
#5091=VERTEX_POINT('',#17255);
#5092=VERTEX_POINT('',#17257);
#5093=VERTEX_POINT('',#17259);
#5094=VERTEX_POINT('',#17261);
#5095=VERTEX_POINT('',#17263);
#5096=VERTEX_POINT('',#17265);
#5097=VERTEX_POINT('',#17267);
#5098=VERTEX_POINT('',#17269);
#5099=VERTEX_POINT('',#17271);
#5100=VERTEX_POINT('',#17273);
#5101=VERTEX_POINT('',#17275);
#5102=VERTEX_POINT('',#17277);
#5103=VERTEX_POINT('',#17279);
#5104=VERTEX_POINT('',#17281);
#5105=VERTEX_POINT('',#17283);
#5106=VERTEX_POINT('',#17285);
#5107=VERTEX_POINT('',#17287);
#5108=VERTEX_POINT('',#17289);
#5109=VERTEX_POINT('',#17291);
#5110=VERTEX_POINT('',#17293);
#5111=VERTEX_POINT('',#17295);
#5112=VERTEX_POINT('',#17297);
#5113=VERTEX_POINT('',#17299);
#5114=VERTEX_POINT('',#17301);
#5115=VERTEX_POINT('',#17303);
#5116=VERTEX_POINT('',#17305);
#5117=VERTEX_POINT('',#17307);
#5118=VERTEX_POINT('',#17309);
#5119=VERTEX_POINT('',#17311);
#5120=VERTEX_POINT('',#17313);
#5121=VERTEX_POINT('',#17315);
#5122=VERTEX_POINT('',#17317);
#5123=VERTEX_POINT('',#17319);
#5124=VERTEX_POINT('',#17321);
#5125=VERTEX_POINT('',#17323);
#5126=VERTEX_POINT('',#17325);
#5127=VERTEX_POINT('',#17327);
#5128=VERTEX_POINT('',#17329);
#5129=VERTEX_POINT('',#17331);
#5130=VERTEX_POINT('',#17333);
#5131=VERTEX_POINT('',#17335);
#5132=VERTEX_POINT('',#17337);
#5133=VERTEX_POINT('',#17339);
#5134=VERTEX_POINT('',#17341);
#5135=VERTEX_POINT('',#17343);
#5136=VERTEX_POINT('',#17345);
#5137=VERTEX_POINT('',#17347);
#5138=VERTEX_POINT('',#17349);
#5139=VERTEX_POINT('',#17351);
#5140=VERTEX_POINT('',#17353);
#5141=VERTEX_POINT('',#17355);
#5142=VERTEX_POINT('',#17357);
#5143=VERTEX_POINT('',#17359);
#5144=VERTEX_POINT('',#17361);
#5145=VERTEX_POINT('',#17363);
#5146=VERTEX_POINT('',#17365);
#5147=VERTEX_POINT('',#17367);
#5148=VERTEX_POINT('',#17369);
#5149=VERTEX_POINT('',#17371);
#5150=VERTEX_POINT('',#17373);
#5151=VERTEX_POINT('',#17375);
#5152=VERTEX_POINT('',#17377);
#5153=VERTEX_POINT('',#17379);
#5154=VERTEX_POINT('',#17381);
#5155=VERTEX_POINT('',#17383);
#5156=VERTEX_POINT('',#17385);
#5157=VERTEX_POINT('',#17387);
#5158=VERTEX_POINT('',#17389);
#5159=VERTEX_POINT('',#17391);
#5160=VERTEX_POINT('',#17393);
#5161=VERTEX_POINT('',#17395);
#5162=VERTEX_POINT('',#17397);
#5163=VERTEX_POINT('',#17399);
#5164=VERTEX_POINT('',#17401);
#5165=VERTEX_POINT('',#17403);
#5166=VERTEX_POINT('',#17405);
#5167=VERTEX_POINT('',#17407);
#5168=VERTEX_POINT('',#17409);
#5169=VERTEX_POINT('',#17411);
#5170=VERTEX_POINT('',#17413);
#5171=VERTEX_POINT('',#17415);
#5172=VERTEX_POINT('',#17417);
#5173=VERTEX_POINT('',#17419);
#5174=VERTEX_POINT('',#17421);
#5175=VERTEX_POINT('',#17423);
#5176=VERTEX_POINT('',#17425);
#5177=VERTEX_POINT('',#17427);
#5178=VERTEX_POINT('',#17429);
#5179=VERTEX_POINT('',#17431);
#5180=VERTEX_POINT('',#17434);
#5181=VERTEX_POINT('',#17435);
#5182=VERTEX_POINT('',#17437);
#5183=VERTEX_POINT('',#17439);
#5184=VERTEX_POINT('',#17441);
#5185=VERTEX_POINT('',#17443);
#5186=VERTEX_POINT('',#17445);
#5187=VERTEX_POINT('',#17447);
#5188=VERTEX_POINT('',#17450);
#5189=VERTEX_POINT('',#17451);
#5190=VERTEX_POINT('',#17453);
#5191=VERTEX_POINT('',#17455);
#5192=VERTEX_POINT('',#17457);
#5193=VERTEX_POINT('',#17459);
#5194=VERTEX_POINT('',#17461);
#5195=VERTEX_POINT('',#17463);
#5196=VERTEX_POINT('',#17465);
#5197=VERTEX_POINT('',#17467);
#5198=VERTEX_POINT('',#17469);
#5199=VERTEX_POINT('',#17471);
#5200=VERTEX_POINT('',#17473);
#5201=VERTEX_POINT('',#17476);
#5202=VERTEX_POINT('',#17479);
#5203=VERTEX_POINT('',#17480);
#5204=VERTEX_POINT('',#17482);
#5205=VERTEX_POINT('',#17484);
#5206=VERTEX_POINT('',#17486);
#5207=VERTEX_POINT('',#17488);
#5208=VERTEX_POINT('',#17490);
#5209=VERTEX_POINT('',#17492);
#5210=VERTEX_POINT('',#17495);
#5211=VERTEX_POINT('',#17496);
#5212=VERTEX_POINT('',#17498);
#5213=VERTEX_POINT('',#17500);
#5214=VERTEX_POINT('',#17502);
#5215=VERTEX_POINT('',#17504);
#5216=VERTEX_POINT('',#17506);
#5217=VERTEX_POINT('',#17508);
#5218=VERTEX_POINT('',#17511);
#5219=VERTEX_POINT('',#17512);
#5220=VERTEX_POINT('',#17514);
#5221=VERTEX_POINT('',#17516);
#5222=VERTEX_POINT('',#17518);
#5223=VERTEX_POINT('',#17520);
#5224=VERTEX_POINT('',#17522);
#5225=VERTEX_POINT('',#17524);
#5226=VERTEX_POINT('',#17528);
#5227=VERTEX_POINT('',#17529);
#5228=VERTEX_POINT('',#17531);
#5229=VERTEX_POINT('',#17533);
#5230=VERTEX_POINT('',#17535);
#5231=VERTEX_POINT('',#17537);
#5232=VERTEX_POINT('',#17539);
#5233=VERTEX_POINT('',#17541);
#5234=VERTEX_POINT('',#17543);
#5235=VERTEX_POINT('',#17545);
#5236=VERTEX_POINT('',#17547);
#5237=VERTEX_POINT('',#17549);
#5238=VERTEX_POINT('',#17551);
#5239=VERTEX_POINT('',#17553);
#5240=VERTEX_POINT('',#17555);
#5241=VERTEX_POINT('',#17557);
#5242=VERTEX_POINT('',#17559);
#5243=VERTEX_POINT('',#17561);
#5244=VERTEX_POINT('',#17563);
#5245=VERTEX_POINT('',#17565);
#5246=VERTEX_POINT('',#17567);
#5247=VERTEX_POINT('',#17569);
#5248=VERTEX_POINT('',#17571);
#5249=VERTEX_POINT('',#17573);
#5250=VERTEX_POINT('',#17575);
#5251=VERTEX_POINT('',#17577);
#5252=VERTEX_POINT('',#17579);
#5253=VERTEX_POINT('',#17581);
#5254=VERTEX_POINT('',#17583);
#5255=VERTEX_POINT('',#17585);
#5256=VERTEX_POINT('',#17587);
#5257=VERTEX_POINT('',#17589);
#5258=VERTEX_POINT('',#17591);
#5259=VERTEX_POINT('',#17593);
#5260=VERTEX_POINT('',#17595);
#5261=VERTEX_POINT('',#17597);
#5262=VERTEX_POINT('',#17599);
#5263=VERTEX_POINT('',#17601);
#5264=VERTEX_POINT('',#17603);
#5265=VERTEX_POINT('',#17605);
#5266=VERTEX_POINT('',#17607);
#5267=VERTEX_POINT('',#17609);
#5268=VERTEX_POINT('',#17611);
#5269=VERTEX_POINT('',#17613);
#5270=VERTEX_POINT('',#17615);
#5271=VERTEX_POINT('',#17617);
#5272=VERTEX_POINT('',#17619);
#5273=VERTEX_POINT('',#17621);
#5274=VERTEX_POINT('',#17623);
#5275=VERTEX_POINT('',#17625);
#5276=VERTEX_POINT('',#17627);
#5277=VERTEX_POINT('',#17629);
#5278=VERTEX_POINT('',#17631);
#5279=VERTEX_POINT('',#17633);
#5280=VERTEX_POINT('',#17635);
#5281=VERTEX_POINT('',#17637);
#5282=VERTEX_POINT('',#17639);
#5283=VERTEX_POINT('',#17641);
#5284=VERTEX_POINT('',#17643);
#5285=VERTEX_POINT('',#17645);
#5286=VERTEX_POINT('',#17647);
#5287=VERTEX_POINT('',#17649);
#5288=VERTEX_POINT('',#17651);
#5289=VERTEX_POINT('',#17653);
#5290=VERTEX_POINT('',#17655);
#5291=VERTEX_POINT('',#17657);
#5292=VERTEX_POINT('',#17659);
#5293=VERTEX_POINT('',#17661);
#5294=VERTEX_POINT('',#17663);
#5295=VERTEX_POINT('',#17665);
#5296=VERTEX_POINT('',#17667);
#5297=VERTEX_POINT('',#17669);
#5298=VERTEX_POINT('',#17671);
#5299=VERTEX_POINT('',#17673);
#5300=VERTEX_POINT('',#17675);
#5301=VERTEX_POINT('',#17677);
#5302=VERTEX_POINT('',#17679);
#5303=VERTEX_POINT('',#17681);
#5304=VERTEX_POINT('',#17683);
#5305=VERTEX_POINT('',#17685);
#5306=VERTEX_POINT('',#17687);
#5307=VERTEX_POINT('',#17689);
#5308=VERTEX_POINT('',#17691);
#5309=VERTEX_POINT('',#17693);
#5310=VERTEX_POINT('',#17695);
#5311=VERTEX_POINT('',#17697);
#5312=VERTEX_POINT('',#17699);
#5313=VERTEX_POINT('',#17701);
#5314=VERTEX_POINT('',#17703);
#5315=VERTEX_POINT('',#17705);
#5316=VERTEX_POINT('',#17707);
#5317=VERTEX_POINT('',#17709);
#5318=VERTEX_POINT('',#17711);
#5319=VERTEX_POINT('',#17713);
#5320=VERTEX_POINT('',#17715);
#5321=VERTEX_POINT('',#17717);
#5322=VERTEX_POINT('',#17719);
#5323=VERTEX_POINT('',#17721);
#5324=VERTEX_POINT('',#17723);
#5325=VERTEX_POINT('',#17725);
#5326=VERTEX_POINT('',#17727);
#5327=VERTEX_POINT('',#17729);
#5328=VERTEX_POINT('',#17731);
#5329=VERTEX_POINT('',#17733);
#5330=VERTEX_POINT('',#17735);
#5331=VERTEX_POINT('',#17737);
#5332=VERTEX_POINT('',#17739);
#5333=VERTEX_POINT('',#17741);
#5334=VERTEX_POINT('',#17743);
#5335=VERTEX_POINT('',#17745);
#5336=VERTEX_POINT('',#17747);
#5337=VERTEX_POINT('',#17749);
#5338=VERTEX_POINT('',#17751);
#5339=VERTEX_POINT('',#17753);
#5340=VERTEX_POINT('',#17755);
#5341=VERTEX_POINT('',#17757);
#5342=VERTEX_POINT('',#17760);
#5343=VERTEX_POINT('',#17761);
#5344=VERTEX_POINT('',#17763);
#5345=VERTEX_POINT('',#17765);
#5346=VERTEX_POINT('',#17767);
#5347=VERTEX_POINT('',#17769);
#5348=VERTEX_POINT('',#17771);
#5349=VERTEX_POINT('',#17773);
#5350=VERTEX_POINT('',#17776);
#5351=VERTEX_POINT('',#17777);
#5352=VERTEX_POINT('',#17779);
#5353=VERTEX_POINT('',#17781);
#5354=VERTEX_POINT('',#17783);
#5355=VERTEX_POINT('',#17785);
#5356=VERTEX_POINT('',#17787);
#5357=VERTEX_POINT('',#17789);
#5358=VERTEX_POINT('',#17792);
#5359=VERTEX_POINT('',#17793);
#5360=VERTEX_POINT('',#17795);
#5361=VERTEX_POINT('',#17797);
#5362=VERTEX_POINT('',#17799);
#5363=VERTEX_POINT('',#17801);
#5364=VERTEX_POINT('',#17803);
#5365=VERTEX_POINT('',#17805);
#5366=VERTEX_POINT('',#17808);
#5367=VERTEX_POINT('',#17809);
#5368=VERTEX_POINT('',#17811);
#5369=VERTEX_POINT('',#17813);
#5370=VERTEX_POINT('',#17815);
#5371=VERTEX_POINT('',#17817);
#5372=VERTEX_POINT('',#17819);
#5373=VERTEX_POINT('',#17821);
#5374=VERTEX_POINT('',#17824);
#5375=VERTEX_POINT('',#17825);
#5376=VERTEX_POINT('',#17827);
#5377=VERTEX_POINT('',#17829);
#5378=VERTEX_POINT('',#17832);
#5379=VERTEX_POINT('',#17834);
#5380=VERTEX_POINT('',#17836);
#5381=VERTEX_POINT('',#17838);
#5382=VERTEX_POINT('',#17840);
#5383=VERTEX_POINT('',#17842);
#5384=VERTEX_POINT('',#17844);
#5385=VERTEX_POINT('',#17846);
#5386=VERTEX_POINT('',#17848);
#5387=VERTEX_POINT('',#17850);
#5388=VERTEX_POINT('',#18180);
#5389=VERTEX_POINT('',#18182);
#5390=VERTEX_POINT('',#18186);
#5391=VERTEX_POINT('',#18188);
#5392=VERTEX_POINT('',#18192);
#5393=VERTEX_POINT('',#18193);
#5394=VERTEX_POINT('',#18195);
#5395=VERTEX_POINT('',#18197);
#5396=VERTEX_POINT('',#18199);
#5397=VERTEX_POINT('',#18203);
#5398=VERTEX_POINT('',#18204);
#5399=VERTEX_POINT('',#18206);
#5400=VERTEX_POINT('',#18208);
#5401=VERTEX_POINT('',#18210);
#5402=VERTEX_POINT('',#18214);
#5403=VERTEX_POINT('',#18215);
#5404=VERTEX_POINT('',#18217);
#5405=VERTEX_POINT('',#18219);
#5406=VERTEX_POINT('',#18221);
#5407=VERTEX_POINT('',#18225);
#5408=VERTEX_POINT('',#18227);
#5409=VERTEX_POINT('',#18230);
#5410=VERTEX_POINT('',#18232);
#5411=VERTEX_POINT('',#18236);
#5412=VERTEX_POINT('',#18238);
#5413=VERTEX_POINT('',#18240);
#5414=VERTEX_POINT('',#18242);
#5415=VERTEX_POINT('',#18246);
#5416=VERTEX_POINT('',#18247);
#5417=VERTEX_POINT('',#18249);
#5418=VERTEX_POINT('',#18251);
#5419=VERTEX_POINT('',#18253);
#5420=VERTEX_POINT('',#18255);
#5421=VERTEX_POINT('',#18257);
#5422=VERTEX_POINT('',#18259);
#5423=VERTEX_POINT('',#18263);
#5424=VERTEX_POINT('',#18264);
#5425=VERTEX_POINT('',#18266);
#5426=VERTEX_POINT('',#18268);
#5427=VERTEX_POINT('',#18270);
#5428=VERTEX_POINT('',#18274);
#5429=VERTEX_POINT('',#18275);
#5430=VERTEX_POINT('',#18278);
#5431=VERTEX_POINT('',#18280);
#5432=VERTEX_POINT('',#18285);
#5433=VERTEX_POINT('',#18286);
#5434=VERTEX_POINT('',#18289);
#5435=VERTEX_POINT('',#18291);
#5436=VERTEX_POINT('',#18295);
#5437=VERTEX_POINT('',#18296);
#5438=VERTEX_POINT('',#18298);
#5439=VERTEX_POINT('',#18300);
#5440=VERTEX_POINT('',#18302);
#5441=VERTEX_POINT('',#18304);
#5442=VERTEX_POINT('',#18306);
#5443=VERTEX_POINT('',#18308);
#5444=VERTEX_POINT('',#18318);
#5445=VERTEX_POINT('',#18319);
#5446=VERTEX_POINT('',#18321);
#5447=VERTEX_POINT('',#18323);
#5448=VERTEX_POINT('',#18333);
#5449=VERTEX_POINT('',#18334);
#5450=VERTEX_POINT('',#18336);
#5451=VERTEX_POINT('',#18338);
#5452=VERTEX_POINT('',#18357);
#5453=VERTEX_POINT('',#18361);
#5454=VERTEX_POINT('',#18369);
#5455=VERTEX_POINT('',#18373);
#5456=VERTEX_POINT('',#18387);
#5457=VERTEX_POINT('',#18389);
#5458=VERTEX_POINT('',#18393);
#5459=VERTEX_POINT('',#18395);
#5460=VERTEX_POINT('',#18399);
#5461=VERTEX_POINT('',#18400);
#5462=VERTEX_POINT('',#18402);
#5463=VERTEX_POINT('',#18404);
#5464=VERTEX_POINT('',#18406);
#5465=VERTEX_POINT('',#18408);
#5466=VERTEX_POINT('',#18412);
#5467=VERTEX_POINT('',#18413);
#5468=VERTEX_POINT('',#18415);
#5469=VERTEX_POINT('',#18417);
#5470=VERTEX_POINT('',#18419);
#5471=VERTEX_POINT('',#18421);
#5472=VERTEX_POINT('',#18423);
#5473=VERTEX_POINT('',#18425);
#5474=VERTEX_POINT('',#18429);
#5475=VERTEX_POINT('',#18431);
#5476=VERTEX_POINT('',#18435);
#5477=VERTEX_POINT('',#18437);
#5478=VERTEX_POINT('',#18441);
#5479=VERTEX_POINT('',#18444);
#5480=VERTEX_POINT('',#18446);
#5481=VERTEX_POINT('',#18450);
#5482=VERTEX_POINT('',#18453);
#5483=VERTEX_POINT('',#18455);
#5484=VERTEX_POINT('',#18459);
#5485=VERTEX_POINT('',#18461);
#5486=VERTEX_POINT('',#18466);
#5487=VERTEX_POINT('',#18468);
#5488=VERTEX_POINT('',#18487);
#5489=VERTEX_POINT('',#18488);
#5490=VERTEX_POINT('',#18490);
#5491=VERTEX_POINT('',#18492);
#5492=VERTEX_POINT('',#18494);
#5493=VERTEX_POINT('',#18496);
#5494=VERTEX_POINT('',#18498);
#5495=VERTEX_POINT('',#18500);
#5496=VERTEX_POINT('',#18503);
#5497=VERTEX_POINT('',#18504);
#5498=VERTEX_POINT('',#18506);
#5499=VERTEX_POINT('',#18508);
#5500=VERTEX_POINT('',#18512);
#5501=VERTEX_POINT('',#18513);
#5502=VERTEX_POINT('',#18515);
#5503=VERTEX_POINT('',#18517);
#5504=VERTEX_POINT('',#18519);
#5505=VERTEX_POINT('',#18521);
#5506=VERTEX_POINT('',#18523);
#5507=VERTEX_POINT('',#18525);
#5508=VERTEX_POINT('',#18528);
#5509=VERTEX_POINT('',#18529);
#5510=VERTEX_POINT('',#18531);
#5511=VERTEX_POINT('',#18533);
#5512=VERTEX_POINT('',#18562);
#5513=VERTEX_POINT('',#18564);
#5514=VERTEX_POINT('',#18568);
#5515=VERTEX_POINT('',#18569);
#5516=VERTEX_POINT('',#18572);
#5517=VERTEX_POINT('',#18576);
#5518=VERTEX_POINT('',#18580);
#5519=VERTEX_POINT('',#18582);
#5520=VERTEX_POINT('',#18586);
#5521=VERTEX_POINT('',#18588);
#5522=VERTEX_POINT('',#18592);
#5523=VERTEX_POINT('',#18594);
#5524=VERTEX_POINT('',#18598);
#5525=VERTEX_POINT('',#18600);
#5526=VERTEX_POINT('',#18611);
#5527=VERTEX_POINT('',#18612);
#5528=VERTEX_POINT('',#18615);
#5529=VERTEX_POINT('',#18616);
#5530=VERTEX_POINT('',#18619);
#5531=VERTEX_POINT('',#18620);
#5532=VERTEX_POINT('',#18623);
#5533=VERTEX_POINT('',#18624);
#5534=VERTEX_POINT('',#18627);
#5535=VERTEX_POINT('',#18628);
#5536=VERTEX_POINT('',#18631);
#5537=VERTEX_POINT('',#18632);
#5538=VERTEX_POINT('',#18635);
#5539=VERTEX_POINT('',#18636);
#5540=VERTEX_POINT('',#18639);
#5541=VERTEX_POINT('',#18641);
#5542=VERTEX_POINT('',#18645);
#5543=VERTEX_POINT('',#18649);
#5544=VERTEX_POINT('',#18653);
#5545=VERTEX_POINT('',#18655);
#5546=VERTEX_POINT('',#18659);
#5547=VERTEX_POINT('',#18663);
#5548=VERTEX_POINT('',#18667);
#5549=VERTEX_POINT('',#18671);
#5550=VERTEX_POINT('',#18675);
#5551=VERTEX_POINT('',#18676);
#5552=VERTEX_POINT('',#18681);
#5553=VERTEX_POINT('',#18683);
#5554=VERTEX_POINT('',#18687);
#5555=VERTEX_POINT('',#18691);
#5556=VERTEX_POINT('',#18697);
#5557=VERTEX_POINT('',#18699);
#5558=VERTEX_POINT('',#18703);
#5559=VERTEX_POINT('',#18705);
#5560=VERTEX_POINT('',#18709);
#5561=VERTEX_POINT('',#18713);
#5562=VERTEX_POINT('',#18714);
#5563=VERTEX_POINT('',#18719);
#5564=VERTEX_POINT('',#18723);
#5565=VERTEX_POINT('',#18724);
#5566=VERTEX_POINT('',#18726);
#5567=VERTEX_POINT('',#18731);
#5568=VERTEX_POINT('',#18732);
#5569=VERTEX_POINT('',#18734);
#5570=VERTEX_POINT('',#18739);
#5571=VERTEX_POINT('',#18741);
#5572=VERTEX_POINT('',#18745);
#5573=VERTEX_POINT('',#18746);
#5574=VERTEX_POINT('',#18749);
#5575=VERTEX_POINT('',#18753);
#5576=VERTEX_POINT('',#18755);
#5577=VERTEX_POINT('',#18763);
#5578=VERTEX_POINT('',#18765);
#5579=VERTEX_POINT('',#18769);
#5580=VERTEX_POINT('',#18773);
#5581=VERTEX_POINT('',#18775);
#5582=VERTEX_POINT('',#18779);
#5583=VERTEX_POINT('',#18783);
#5584=VERTEX_POINT('',#18787);
#5585=VERTEX_POINT('',#18789);
#5586=VERTEX_POINT('',#18793);
#5587=EDGE_CURVE('',#4574,#4574,#4075,.T.);
#5588=EDGE_CURVE('',#4574,#4575,#2047,.T.);
#5589=EDGE_CURVE('',#4575,#4575,#4076,.T.);
#5590=EDGE_CURVE('',#4576,#4576,#4077,.T.);
#5591=EDGE_CURVE('',#4576,#4577,#2048,.T.);
#5592=EDGE_CURVE('',#4577,#4577,#4078,.T.);
#5593=EDGE_CURVE('',#4578,#4578,#4079,.T.);
#5594=EDGE_CURVE('',#4578,#4579,#2049,.T.);
#5595=EDGE_CURVE('',#4579,#4579,#4080,.T.);
#5596=EDGE_CURVE('',#4580,#4580,#4081,.T.);
#5597=EDGE_CURVE('',#4580,#4581,#2050,.T.);
#5598=EDGE_CURVE('',#4581,#4581,#4082,.T.);
#5599=EDGE_CURVE('',#4582,#4582,#4083,.T.);
#5600=EDGE_CURVE('',#4582,#4583,#2051,.T.);
#5601=EDGE_CURVE('',#4583,#4583,#4084,.T.);
#5602=EDGE_CURVE('',#4584,#4584,#4085,.T.);
#5603=EDGE_CURVE('',#4584,#4585,#2052,.T.);
#5604=EDGE_CURVE('',#4585,#4585,#4086,.T.);
#5605=EDGE_CURVE('',#4586,#4586,#4087,.T.);
#5606=EDGE_CURVE('',#4586,#4587,#2053,.T.);
#5607=EDGE_CURVE('',#4587,#4587,#4088,.T.);
#5608=EDGE_CURVE('',#4588,#4588,#4089,.T.);
#5609=EDGE_CURVE('',#4588,#4589,#2054,.T.);
#5610=EDGE_CURVE('',#4589,#4589,#4090,.T.);
#5611=EDGE_CURVE('',#4590,#4590,#4091,.T.);
#5612=EDGE_CURVE('',#4590,#4591,#2055,.T.);
#5613=EDGE_CURVE('',#4591,#4591,#4092,.T.);
#5614=EDGE_CURVE('',#4592,#4593,#2056,.T.);
#5615=EDGE_CURVE('',#4594,#4592,#2057,.T.);
#5616=EDGE_CURVE('',#4594,#4595,#2058,.T.);
#5617=EDGE_CURVE('',#4595,#4596,#2059,.T.);
#5618=EDGE_CURVE('',#4596,#4597,#2060,.T.);
#5619=EDGE_CURVE('',#4598,#4597,#2061,.T.);
#5620=EDGE_CURVE('',#4598,#4599,#2062,.T.);
#5621=EDGE_CURVE('',#4600,#4599,#2063,.T.);
#5622=EDGE_CURVE('',#4600,#4601,#2064,.T.);
#5623=EDGE_CURVE('',#4601,#4593,#2065,.T.);
#5624=EDGE_CURVE('',#4593,#4602,#2066,.T.);
#5625=EDGE_CURVE('',#4601,#4603,#2067,.T.);
#5626=EDGE_CURVE('',#4603,#4604,#4093,.T.);
#5627=EDGE_CURVE('',#4604,#4602,#2068,.T.);
#5628=EDGE_CURVE('',#4605,#4595,#2069,.T.);
#5629=EDGE_CURVE('',#4605,#4606,#2070,.T.);
#5630=EDGE_CURVE('',#4606,#4607,#4094,.T.);
#5631=EDGE_CURVE('',#4596,#4607,#2071,.T.);
#5632=EDGE_CURVE('',#4608,#4609,#2072,.T.);
#5633=EDGE_CURVE('',#4609,#4610,#2073,.T.);
#5634=EDGE_CURVE('',#4610,#4611,#2074,.T.);
#5635=EDGE_CURVE('',#4611,#4612,#2075,.T.);
#5636=EDGE_CURVE('',#4613,#4612,#4095,.T.);
#5637=EDGE_CURVE('',#4613,#4600,#2076,.T.);
#5638=EDGE_CURVE('',#4614,#4599,#2077,.T.);
#5639=EDGE_CURVE('',#4608,#4614,#2078,.T.);
#5640=EDGE_CURVE('',#4615,#4616,#2079,.T.);
#5641=EDGE_CURVE('',#4617,#4615,#2080,.T.);
#5642=EDGE_CURVE('',#4618,#4617,#2081,.T.);
#5643=EDGE_CURVE('',#4619,#4618,#2082,.T.);
#5644=EDGE_CURVE('',#4620,#4619,#2083,.T.);
#5645=EDGE_CURVE('',#4616,#4620,#2084,.T.);
#5646=EDGE_CURVE('',#4621,#4622,#2085,.T.);
#5647=EDGE_CURVE('',#4623,#4621,#2086,.T.);
#5648=EDGE_CURVE('',#4624,#4623,#2087,.T.);
#5649=EDGE_CURVE('',#4625,#4624,#2088,.T.);
#5650=EDGE_CURVE('',#4626,#4625,#2089,.T.);
#5651=EDGE_CURVE('',#4622,#4626,#2090,.T.);
#5652=EDGE_CURVE('',#4627,#4613,#2091,.T.);
#5653=EDGE_CURVE('',#4627,#4628,#2092,.T.);
#5654=EDGE_CURVE('',#4628,#4601,#2093,.T.);
#5655=EDGE_CURVE('',#4629,#4612,#2094,.T.);
#5656=EDGE_CURVE('',#4627,#4629,#4096,.T.);
#5657=EDGE_CURVE('',#4607,#4630,#2095,.T.);
#5658=EDGE_CURVE('',#4630,#4629,#2096,.T.);
#5659=EDGE_CURVE('',#4611,#4631,#2097,.T.);
#5660=EDGE_CURVE('',#4631,#4597,#2098,.T.);
#5661=EDGE_CURVE('',#4632,#4606,#2099,.T.);
#5662=EDGE_CURVE('',#4633,#4605,#2100,.T.);
#5663=EDGE_CURVE('',#4634,#4633,#2101,.T.);
#5664=EDGE_CURVE('',#4634,#4602,#2102,.T.);
#5665=EDGE_CURVE('',#4604,#4635,#2103,.T.);
#5666=EDGE_CURVE('',#4632,#4635,#2104,.T.);
#5667=EDGE_CURVE('',#4636,#4603,#2105,.T.);
#5668=EDGE_CURVE('',#4636,#4628,#2106,.T.);
#5669=EDGE_CURVE('',#4635,#4636,#4097,.T.);
#5670=EDGE_CURVE('',#4630,#4632,#4098,.T.);
#5671=EDGE_CURVE('',#4637,#4598,#2107,.T.);
#5672=EDGE_CURVE('',#4637,#4614,#2108,.T.);
#5673=EDGE_CURVE('',#4638,#4637,#2109,.T.);
#5674=EDGE_CURVE('',#4638,#4608,#2110,.T.);
#5675=EDGE_CURVE('',#4639,#4631,#2111,.T.);
#5676=EDGE_CURVE('',#4639,#4640,#2112,.T.);
#5677=EDGE_CURVE('',#4640,#4638,#2113,.T.);
#5678=EDGE_CURVE('',#4641,#4621,#2114,.T.);
#5679=EDGE_CURVE('',#4642,#4641,#2115,.T.);
#5680=EDGE_CURVE('',#4642,#4623,#2116,.T.);
#5681=EDGE_CURVE('',#4643,#4642,#2117,.T.);
#5682=EDGE_CURVE('',#4643,#4624,#2118,.T.);
#5683=EDGE_CURVE('',#4644,#4643,#2119,.T.);
#5684=EDGE_CURVE('',#4644,#4625,#2120,.T.);
#5685=EDGE_CURVE('',#4645,#4644,#2121,.T.);
#5686=EDGE_CURVE('',#4645,#4626,#2122,.T.);
#5687=EDGE_CURVE('',#4646,#4645,#2123,.T.);
#5688=EDGE_CURVE('',#4646,#4622,#2124,.T.);
#5689=EDGE_CURVE('',#4641,#4646,#2125,.T.);
#5690=EDGE_CURVE('',#4647,#4615,#2126,.T.);
#5691=EDGE_CURVE('',#4648,#4647,#2127,.T.);
#5692=EDGE_CURVE('',#4648,#4617,#2128,.T.);
#5693=EDGE_CURVE('',#4649,#4648,#2129,.T.);
#5694=EDGE_CURVE('',#4649,#4618,#2130,.T.);
#5695=EDGE_CURVE('',#4650,#4649,#2131,.T.);
#5696=EDGE_CURVE('',#4650,#4619,#2132,.T.);
#5697=EDGE_CURVE('',#4651,#4650,#2133,.T.);
#5698=EDGE_CURVE('',#4651,#4620,#2134,.T.);
#5699=EDGE_CURVE('',#4652,#4651,#2135,.T.);
#5700=EDGE_CURVE('',#4652,#4616,#2136,.T.);
#5701=EDGE_CURVE('',#4647,#4652,#2137,.T.);
#5702=EDGE_CURVE('',#4640,#4609,#2138,.T.);
#5703=EDGE_CURVE('',#4610,#4639,#2139,.T.);
#5704=EDGE_CURVE('',#4592,#4634,#2140,.T.);
#5705=EDGE_CURVE('',#4633,#4594,#2141,.T.);
#5706=EDGE_CURVE('',#4653,#4653,#4099,.T.);
#5707=EDGE_CURVE('',#4653,#4654,#2142,.T.);
#5708=EDGE_CURVE('',#4654,#4654,#4100,.T.);
#5709=EDGE_CURVE('',#4655,#4655,#4101,.T.);
#5710=EDGE_CURVE('',#4655,#4656,#2143,.T.);
#5711=EDGE_CURVE('',#4656,#4656,#4102,.T.);
#5712=EDGE_CURVE('',#4657,#4657,#4103,.T.);
#5713=EDGE_CURVE('',#4657,#4658,#2144,.T.);
#5714=EDGE_CURVE('',#4658,#4658,#4104,.T.);
#5715=EDGE_CURVE('',#4659,#4659,#4105,.T.);
#5716=EDGE_CURVE('',#4659,#4660,#2145,.T.);
#5717=EDGE_CURVE('',#4660,#4660,#4106,.T.);
#5718=EDGE_CURVE('',#4661,#4661,#4107,.T.);
#5719=EDGE_CURVE('',#4661,#4662,#2146,.T.);
#5720=EDGE_CURVE('',#4662,#4662,#4108,.T.);
#5721=EDGE_CURVE('',#4663,#4663,#4109,.T.);
#5722=EDGE_CURVE('',#4663,#4664,#2147,.T.);
#5723=EDGE_CURVE('',#4664,#4664,#4110,.T.);
#5724=EDGE_CURVE('',#4665,#4665,#4111,.T.);
#5725=EDGE_CURVE('',#4665,#4666,#2148,.T.);
#5726=EDGE_CURVE('',#4666,#4666,#4112,.T.);
#5727=EDGE_CURVE('',#4667,#4667,#4113,.T.);
#5728=EDGE_CURVE('',#4667,#4668,#2149,.T.);
#5729=EDGE_CURVE('',#4668,#4668,#4114,.T.);
#5730=EDGE_CURVE('',#4669,#4669,#4115,.T.);
#5731=EDGE_CURVE('',#4669,#4670,#2150,.T.);
#5732=EDGE_CURVE('',#4670,#4670,#4116,.T.);
#5733=EDGE_CURVE('',#4671,#4672,#2151,.T.);
#5734=EDGE_CURVE('',#4673,#4672,#2152,.T.);
#5735=EDGE_CURVE('',#4674,#4673,#2153,.T.);
#5736=EDGE_CURVE('',#4674,#4675,#2154,.T.);
#5737=EDGE_CURVE('',#4676,#4675,#2155,.T.);
#5738=EDGE_CURVE('',#4676,#4677,#2156,.T.);
#5739=EDGE_CURVE('',#4678,#4677,#2157,.T.);
#5740=EDGE_CURVE('',#4679,#4678,#2158,.T.);
#5741=EDGE_CURVE('',#4680,#4679,#2159,.T.);
#5742=EDGE_CURVE('',#4680,#4671,#2160,.T.);
#5743=EDGE_CURVE('',#4672,#4681,#2161,.T.);
#5744=EDGE_CURVE('',#4682,#4681,#2162,.T.);
#5745=EDGE_CURVE('',#4683,#4682,#4117,.T.);
#5746=EDGE_CURVE('',#4673,#4683,#2163,.T.);
#5747=EDGE_CURVE('',#4684,#4679,#2164,.T.);
#5748=EDGE_CURVE('',#4678,#4685,#2165,.T.);
#5749=EDGE_CURVE('',#4686,#4685,#4118,.T.);
#5750=EDGE_CURVE('',#4684,#4686,#2166,.T.);
#5751=EDGE_CURVE('',#4687,#4688,#2167,.T.);
#5752=EDGE_CURVE('',#4687,#4689,#2168,.T.);
#5753=EDGE_CURVE('',#4689,#4675,#2169,.T.);
#5754=EDGE_CURVE('',#4690,#4674,#2170,.T.);
#5755=EDGE_CURVE('',#4690,#4691,#4119,.T.);
#5756=EDGE_CURVE('',#4692,#4691,#2171,.T.);
#5757=EDGE_CURVE('',#4693,#4692,#2172,.T.);
#5758=EDGE_CURVE('',#4688,#4693,#2173,.T.);
#5759=EDGE_CURVE('',#4694,#4695,#2174,.T.);
#5760=EDGE_CURVE('',#4695,#4696,#2175,.T.);
#5761=EDGE_CURVE('',#4696,#4697,#2176,.T.);
#5762=EDGE_CURVE('',#4697,#4698,#2177,.T.);
#5763=EDGE_CURVE('',#4698,#4699,#2178,.T.);
#5764=EDGE_CURVE('',#4699,#4694,#2179,.T.);
#5765=EDGE_CURVE('',#4700,#4701,#2180,.T.);
#5766=EDGE_CURVE('',#4701,#4702,#2181,.T.);
#5767=EDGE_CURVE('',#4702,#4703,#2182,.T.);
#5768=EDGE_CURVE('',#4703,#4704,#2183,.T.);
#5769=EDGE_CURVE('',#4704,#4705,#2184,.T.);
#5770=EDGE_CURVE('',#4705,#4700,#2185,.T.);
#5771=EDGE_CURVE('',#4706,#4673,#2186,.T.);
#5772=EDGE_CURVE('',#4707,#4706,#2187,.T.);
#5773=EDGE_CURVE('',#4707,#4690,#2188,.T.);
#5774=EDGE_CURVE('',#4707,#4708,#4120,.T.);
#5775=EDGE_CURVE('',#4708,#4691,#2189,.T.);
#5776=EDGE_CURVE('',#4709,#4677,#2190,.T.);
#5777=EDGE_CURVE('',#4692,#4709,#2191,.T.);
#5778=EDGE_CURVE('',#4710,#4708,#2192,.T.);
#5779=EDGE_CURVE('',#4685,#4710,#2193,.T.);
#5780=EDGE_CURVE('',#4711,#4686,#2194,.T.);
#5781=EDGE_CURVE('',#4711,#4712,#2195,.T.);
#5782=EDGE_CURVE('',#4682,#4712,#2196,.T.);
#5783=EDGE_CURVE('',#4713,#4681,#2197,.T.);
#5784=EDGE_CURVE('',#4713,#4714,#2198,.T.);
#5785=EDGE_CURVE('',#4714,#4684,#2199,.T.);
#5786=EDGE_CURVE('',#4715,#4683,#2200,.T.);
#5787=EDGE_CURVE('',#4715,#4706,#2201,.T.);
#5788=EDGE_CURVE('',#4710,#4711,#4121,.T.);
#5789=EDGE_CURVE('',#4712,#4715,#4122,.T.);
#5790=EDGE_CURVE('',#4716,#4689,#2202,.T.);
#5791=EDGE_CURVE('',#4716,#4676,#2203,.T.);
#5792=EDGE_CURVE('',#4717,#4716,#2204,.T.);
#5793=EDGE_CURVE('',#4717,#4687,#2205,.T.);
#5794=EDGE_CURVE('',#4718,#4709,#2206,.T.);
#5795=EDGE_CURVE('',#4719,#4717,#2207,.T.);
#5796=EDGE_CURVE('',#4718,#4719,#2208,.T.);
#5797=EDGE_CURVE('',#4720,#4705,#2209,.T.);
#5798=EDGE_CURVE('',#4720,#4721,#2210,.T.);
#5799=EDGE_CURVE('',#4721,#4700,#2211,.T.);
#5800=EDGE_CURVE('',#4722,#4704,#2212,.T.);
#5801=EDGE_CURVE('',#4722,#4720,#2213,.T.);
#5802=EDGE_CURVE('',#4723,#4703,#2214,.T.);
#5803=EDGE_CURVE('',#4723,#4722,#2215,.T.);
#5804=EDGE_CURVE('',#4724,#4702,#2216,.T.);
#5805=EDGE_CURVE('',#4724,#4723,#2217,.T.);
#5806=EDGE_CURVE('',#4725,#4701,#2218,.T.);
#5807=EDGE_CURVE('',#4725,#4724,#2219,.T.);
#5808=EDGE_CURVE('',#4721,#4725,#2220,.T.);
#5809=EDGE_CURVE('',#4726,#4699,#2221,.T.);
#5810=EDGE_CURVE('',#4726,#4727,#2222,.T.);
#5811=EDGE_CURVE('',#4727,#4694,#2223,.T.);
#5812=EDGE_CURVE('',#4728,#4698,#2224,.T.);
#5813=EDGE_CURVE('',#4728,#4726,#2225,.T.);
#5814=EDGE_CURVE('',#4729,#4697,#2226,.T.);
#5815=EDGE_CURVE('',#4729,#4728,#2227,.T.);
#5816=EDGE_CURVE('',#4730,#4696,#2228,.T.);
#5817=EDGE_CURVE('',#4730,#4729,#2229,.T.);
#5818=EDGE_CURVE('',#4731,#4695,#2230,.T.);
#5819=EDGE_CURVE('',#4731,#4730,#2231,.T.);
#5820=EDGE_CURVE('',#4727,#4731,#2232,.T.);
#5821=EDGE_CURVE('',#4719,#4688,#2233,.T.);
#5822=EDGE_CURVE('',#4693,#4718,#2234,.T.);
#5823=EDGE_CURVE('',#4714,#4680,#2235,.T.);
#5824=EDGE_CURVE('',#4671,#4713,#2236,.T.);
#5825=EDGE_CURVE('',#4732,#4732,#4123,.T.);
#5826=EDGE_CURVE('',#4732,#4733,#2237,.T.);
#5827=EDGE_CURVE('',#4734,#4733,#167,.T.);
#5828=EDGE_CURVE('',#4735,#4734,#4124,.T.);
#5829=EDGE_CURVE('',#4733,#4735,#168,.T.);
#5830=EDGE_CURVE('',#4736,#4736,#4125,.T.);
#5831=EDGE_CURVE('',#4736,#4737,#2238,.T.);
#5832=EDGE_CURVE('',#4737,#4737,#4126,.T.);
#5833=EDGE_CURVE('',#4738,#4738,#4127,.T.);
#5834=EDGE_CURVE('',#4738,#4739,#2239,.T.);
#5835=EDGE_CURVE('',#4739,#4739,#4128,.T.);
#5836=EDGE_CURVE('',#4740,#4740,#4129,.T.);
#5837=EDGE_CURVE('',#4740,#4741,#2240,.T.);
#5838=EDGE_CURVE('',#4741,#4741,#4130,.T.);
#5839=EDGE_CURVE('',#4742,#4742,#4131,.T.);
#5840=EDGE_CURVE('',#4742,#4743,#2241,.T.);
#5841=EDGE_CURVE('',#4743,#4743,#4132,.T.);
#5842=EDGE_CURVE('',#4744,#4744,#4133,.T.);
#5843=EDGE_CURVE('',#4744,#4745,#2242,.T.);
#5844=EDGE_CURVE('',#4745,#4745,#4134,.T.);
#5845=EDGE_CURVE('',#4746,#4746,#4135,.T.);
#5846=EDGE_CURVE('',#4746,#4747,#2243,.T.);
#5847=EDGE_CURVE('',#4747,#4747,#4136,.T.);
#5848=EDGE_CURVE('',#4748,#4749,#2244,.T.);
#5849=EDGE_CURVE('',#4749,#4750,#2245,.T.);
#5850=EDGE_CURVE('',#4751,#4750,#2246,.T.);
#5851=EDGE_CURVE('',#4752,#4751,#4137,.T.);
#5852=EDGE_CURVE('',#4748,#4752,#2247,.T.);
#5853=EDGE_CURVE('',#4753,#4754,#2248,.T.);
#5854=EDGE_CURVE('',#4755,#4754,#2249,.T.);
#5855=EDGE_CURVE('',#4756,#4755,#4138,.T.);
#5856=EDGE_CURVE('',#4756,#4757,#2250,.T.);
#5857=EDGE_CURVE('',#4757,#4753,#2251,.T.);
#5858=EDGE_CURVE('',#4758,#4749,#2252,.T.);
#5859=EDGE_CURVE('',#4758,#4759,#2253,.T.);
#5860=EDGE_CURVE('',#4759,#4753,#2254,.T.);
#5861=EDGE_CURVE('',#4757,#4760,#2255,.T.);
#5862=EDGE_CURVE('',#4760,#4761,#2256,.T.);
#5863=EDGE_CURVE('',#4750,#4761,#2257,.T.);
#5864=EDGE_CURVE('',#4762,#4760,#2258,.T.);
#5865=EDGE_CURVE('',#4763,#4757,#2259,.T.);
#5866=EDGE_CURVE('',#4764,#4763,#2260,.T.);
#5867=EDGE_CURVE('',#4764,#4762,#2261,.T.);
#5868=EDGE_CURVE('',#4762,#4765,#4139,.T.);
#5869=EDGE_CURVE('',#4764,#4766,#4140,.T.);
#5870=EDGE_CURVE('',#4766,#4765,#2262,.T.);
#5871=EDGE_CURVE('',#4761,#4765,#2263,.T.);
#5872=EDGE_CURVE('',#4767,#4766,#2264,.T.);
#5873=EDGE_CURVE('',#4751,#4767,#2265,.T.);
#5874=EDGE_CURVE('',#4768,#4752,#2266,.T.);
#5875=EDGE_CURVE('',#4768,#4769,#2267,.T.);
#5876=EDGE_CURVE('',#4770,#4769,#2268,.T.);
#5877=EDGE_CURVE('',#4771,#4770,#4141,.T.);
#5878=EDGE_CURVE('',#4771,#4772,#2269,.T.);
#5879=EDGE_CURVE('',#4773,#4772,#4142,.T.);
#5880=EDGE_CURVE('',#4773,#4774,#2270,.T.);
#5881=EDGE_CURVE('',#4774,#4775,#2271,.T.);
#5882=EDGE_CURVE('',#4755,#4775,#2272,.T.);
#5883=EDGE_CURVE('',#4776,#4754,#2273,.T.);
#5884=EDGE_CURVE('',#4776,#4777,#2274,.T.);
#5885=EDGE_CURVE('',#4777,#4748,#2275,.T.);
#5886=EDGE_CURVE('',#4778,#4756,#2276,.T.);
#5887=EDGE_CURVE('',#4778,#4763,#2277,.T.);
#5888=EDGE_CURVE('',#4779,#4769,#2278,.T.);
#5889=EDGE_CURVE('',#4767,#4768,#4143,.T.);
#5890=EDGE_CURVE('',#4775,#4778,#4144,.T.);
#5891=EDGE_CURVE('',#4774,#4780,#2279,.T.);
#5892=EDGE_CURVE('',#4735,#4780,#2280,.T.);
#5893=EDGE_CURVE('',#4779,#4734,#2281,.T.);
#5894=EDGE_CURVE('',#4781,#4782,#2282,.T.);
#5895=EDGE_CURVE('',#4780,#4782,#2283,.T.);
#5896=EDGE_CURVE('',#4781,#4773,#2284,.T.);
#5897=EDGE_CURVE('',#4783,#4781,#4145,.T.);
#5898=EDGE_CURVE('',#4783,#4784,#2285,.T.);
#5899=EDGE_CURVE('',#4785,#4784,#4146,.T.);
#5900=EDGE_CURVE('',#4785,#4786,#2286,.T.);
#5901=EDGE_CURVE('',#4782,#4786,#2287,.T.);
#5902=EDGE_CURVE('',#4786,#4779,#2288,.T.);
#5903=EDGE_CURVE('',#4770,#4785,#2289,.T.);
#5904=EDGE_CURVE('',#4772,#4783,#2290,.T.);
#5905=EDGE_CURVE('',#4784,#4771,#2291,.T.);
#5906=EDGE_CURVE('',#4759,#4776,#2292,.T.);
#5907=EDGE_CURVE('',#4777,#4758,#2293,.T.);
#5908=EDGE_CURVE('',#4787,#4787,#4147,.T.);
#5909=EDGE_CURVE('',#4787,#4788,#2294,.T.);
#5910=EDGE_CURVE('',#4788,#4789,#169,.T.);
#5911=EDGE_CURVE('',#4789,#4790,#4148,.T.);
#5912=EDGE_CURVE('',#4790,#4788,#170,.T.);
#5913=EDGE_CURVE('',#4791,#4791,#4149,.T.);
#5914=EDGE_CURVE('',#4791,#4792,#2295,.T.);
#5915=EDGE_CURVE('',#4792,#4792,#4150,.T.);
#5916=EDGE_CURVE('',#4793,#4793,#4151,.T.);
#5917=EDGE_CURVE('',#4793,#4794,#2296,.T.);
#5918=EDGE_CURVE('',#4794,#4794,#4152,.T.);
#5919=EDGE_CURVE('',#4795,#4795,#4153,.T.);
#5920=EDGE_CURVE('',#4795,#4796,#2297,.T.);
#5921=EDGE_CURVE('',#4796,#4796,#4154,.T.);
#5922=EDGE_CURVE('',#4797,#4797,#4155,.T.);
#5923=EDGE_CURVE('',#4797,#4798,#2298,.T.);
#5924=EDGE_CURVE('',#4798,#4798,#4156,.T.);
#5925=EDGE_CURVE('',#4799,#4799,#4157,.T.);
#5926=EDGE_CURVE('',#4799,#4800,#2299,.T.);
#5927=EDGE_CURVE('',#4800,#4800,#4158,.T.);
#5928=EDGE_CURVE('',#4801,#4801,#4159,.T.);
#5929=EDGE_CURVE('',#4801,#4802,#2300,.T.);
#5930=EDGE_CURVE('',#4802,#4802,#4160,.T.);
#5931=EDGE_CURVE('',#4803,#4804,#2301,.T.);
#5932=EDGE_CURVE('',#4803,#4805,#2302,.T.);
#5933=EDGE_CURVE('',#4805,#4806,#4161,.T.);
#5934=EDGE_CURVE('',#4806,#4807,#2303,.T.);
#5935=EDGE_CURVE('',#4804,#4807,#2304,.T.);
#5936=EDGE_CURVE('',#4808,#4809,#2305,.T.);
#5937=EDGE_CURVE('',#4810,#4808,#2306,.T.);
#5938=EDGE_CURVE('',#4811,#4810,#2307,.T.);
#5939=EDGE_CURVE('',#4811,#4812,#4162,.T.);
#5940=EDGE_CURVE('',#4812,#4809,#2308,.T.);
#5941=EDGE_CURVE('',#4813,#4804,#2309,.T.);
#5942=EDGE_CURVE('',#4807,#4814,#2310,.T.);
#5943=EDGE_CURVE('',#4815,#4814,#2311,.T.);
#5944=EDGE_CURVE('',#4810,#4815,#2312,.T.);
#5945=EDGE_CURVE('',#4816,#4808,#2313,.T.);
#5946=EDGE_CURVE('',#4813,#4816,#2314,.T.);
#5947=EDGE_CURVE('',#4817,#4815,#2315,.T.);
#5948=EDGE_CURVE('',#4818,#4817,#2316,.T.);
#5949=EDGE_CURVE('',#4818,#4819,#2317,.T.);
#5950=EDGE_CURVE('',#4819,#4810,#2318,.T.);
#5951=EDGE_CURVE('',#4817,#4820,#4163,.T.);
#5952=EDGE_CURVE('',#4821,#4820,#2319,.T.);
#5953=EDGE_CURVE('',#4818,#4821,#4164,.T.);
#5954=EDGE_CURVE('',#4806,#4822,#2320,.T.);
#5955=EDGE_CURVE('',#4822,#4821,#2321,.T.);
#5956=EDGE_CURVE('',#4814,#4820,#2322,.T.);
#5957=EDGE_CURVE('',#4823,#4805,#2323,.T.);
#5958=EDGE_CURVE('',#4824,#4803,#2324,.T.);
#5959=EDGE_CURVE('',#4825,#4824,#2325,.T.);
#5960=EDGE_CURVE('',#4825,#4809,#2326,.T.);
#5961=EDGE_CURVE('',#4812,#4826,#2327,.T.);
#5962=EDGE_CURVE('',#4827,#4826,#2328,.T.);
#5963=EDGE_CURVE('',#4828,#4827,#2329,.T.);
#5964=EDGE_CURVE('',#4828,#4829,#4165,.T.);
#5965=EDGE_CURVE('',#4830,#4829,#2330,.T.);
#5966=EDGE_CURVE('',#4830,#4831,#4166,.T.);
#5967=EDGE_CURVE('',#4831,#4832,#2331,.T.);
#5968=EDGE_CURVE('',#4823,#4832,#2332,.T.);
#5969=EDGE_CURVE('',#4833,#4811,#2333,.T.);
#5970=EDGE_CURVE('',#4833,#4819,#2334,.T.);
#5971=EDGE_CURVE('',#4834,#4832,#2335,.T.);
#5972=EDGE_CURVE('',#4834,#4790,#2336,.T.);
#5973=EDGE_CURVE('',#4789,#4835,#2337,.T.);
#5974=EDGE_CURVE('',#4827,#4835,#2338,.T.);
#5975=EDGE_CURVE('',#4826,#4833,#4167,.T.);
#5976=EDGE_CURVE('',#4822,#4823,#4168,.T.);
#5977=EDGE_CURVE('',#4836,#4837,#2339,.T.);
#5978=EDGE_CURVE('',#4836,#4828,#2340,.T.);
#5979=EDGE_CURVE('',#4835,#4837,#2341,.T.);
#5980=EDGE_CURVE('',#4837,#4838,#2342,.T.);
#5981=EDGE_CURVE('',#4839,#4838,#2343,.T.);
#5982=EDGE_CURVE('',#4839,#4840,#4169,.T.);
#5983=EDGE_CURVE('',#4841,#4840,#2344,.T.);
#5984=EDGE_CURVE('',#4841,#4836,#4170,.T.);
#5985=EDGE_CURVE('',#4831,#4839,#2345,.T.);
#5986=EDGE_CURVE('',#4838,#4834,#2346,.T.);
#5987=EDGE_CURVE('',#4840,#4830,#2347,.T.);
#5988=EDGE_CURVE('',#4829,#4841,#2348,.T.);
#5989=EDGE_CURVE('',#4824,#4813,#2349,.T.);
#5990=EDGE_CURVE('',#4816,#4825,#2350,.T.);
#5991=EDGE_CURVE('',#4842,#4842,#4171,.T.);
#5992=EDGE_CURVE('',#4842,#4843,#2351,.T.);
#5993=EDGE_CURVE('',#4843,#4843,#4172,.T.);
#5994=EDGE_CURVE('',#4844,#4844,#4173,.T.);
#5995=EDGE_CURVE('',#4844,#4845,#2352,.T.);
#5996=EDGE_CURVE('',#4845,#4845,#4174,.T.);
#5997=EDGE_CURVE('',#4846,#4846,#4175,.T.);
#5998=EDGE_CURVE('',#4846,#4847,#2353,.T.);
#5999=EDGE_CURVE('',#4847,#4847,#4176,.T.);
#6000=EDGE_CURVE('',#4848,#4848,#4177,.T.);
#6001=EDGE_CURVE('',#4848,#4849,#2354,.T.);
#6002=EDGE_CURVE('',#4849,#4849,#4178,.T.);
#6003=EDGE_CURVE('',#4850,#4850,#4179,.T.);
#6004=EDGE_CURVE('',#4850,#4851,#2355,.T.);
#6005=EDGE_CURVE('',#4851,#4851,#4180,.T.);
#6006=EDGE_CURVE('',#4852,#4852,#4181,.T.);
#6007=EDGE_CURVE('',#4852,#4853,#2356,.T.);
#6008=EDGE_CURVE('',#4853,#4853,#4182,.T.);
#6009=EDGE_CURVE('',#4854,#4854,#4183,.T.);
#6010=EDGE_CURVE('',#4854,#4855,#2357,.T.);
#6011=EDGE_CURVE('',#4855,#4855,#4184,.T.);
#6012=EDGE_CURVE('',#4856,#4856,#4185,.T.);
#6013=EDGE_CURVE('',#4856,#4857,#2358,.T.);
#6014=EDGE_CURVE('',#4857,#4857,#4186,.T.);
#6015=EDGE_CURVE('',#4858,#4858,#4187,.T.);
#6016=EDGE_CURVE('',#4858,#4859,#2359,.T.);
#6017=EDGE_CURVE('',#4859,#4859,#4188,.T.);
#6018=EDGE_CURVE('',#4860,#4860,#4189,.T.);
#6019=EDGE_CURVE('',#4860,#4861,#2360,.T.);
#6020=EDGE_CURVE('',#4861,#4861,#4190,.T.);
#6021=EDGE_CURVE('',#4862,#4863,#2361,.T.);
#6022=EDGE_CURVE('',#4862,#4864,#2362,.T.);
#6023=EDGE_CURVE('',#4865,#4864,#2363,.T.);
#6024=EDGE_CURVE('',#4865,#4863,#2364,.T.);
#6025=EDGE_CURVE('',#4866,#4867,#2365,.T.);
#6026=EDGE_CURVE('',#4866,#4868,#2366,.T.);
#6027=EDGE_CURVE('',#4869,#4868,#2367,.T.);
#6028=EDGE_CURVE('',#4869,#4867,#2368,.T.);
#6029=EDGE_CURVE('',#4870,#4871,#2369,.T.);
#6030=EDGE_CURVE('',#4870,#4872,#2370,.T.);
#6031=EDGE_CURVE('',#4873,#4872,#2371,.T.);
#6032=EDGE_CURVE('',#4873,#4871,#2372,.T.);
#6033=EDGE_CURVE('',#4871,#4866,#4191,.T.);
#6034=EDGE_CURVE('',#4868,#4873,#4192,.T.);
#6035=EDGE_CURVE('',#4867,#4862,#4193,.T.);
#6036=EDGE_CURVE('',#4864,#4869,#4194,.T.);
#6037=EDGE_CURVE('',#4874,#4875,#2373,.T.);
#6038=EDGE_CURVE('',#4874,#4876,#2374,.T.);
#6039=EDGE_CURVE('',#4876,#4877,#2375,.T.);
#6040=EDGE_CURVE('',#4875,#4877,#2376,.T.);
#6041=EDGE_CURVE('',#4878,#4876,#4195,.T.);
#6042=EDGE_CURVE('',#4878,#4879,#2377,.T.);
#6043=EDGE_CURVE('',#4879,#4877,#4196,.T.);
#6044=EDGE_CURVE('',#4878,#4880,#2378,.T.);
#6045=EDGE_CURVE('',#4880,#4881,#2379,.T.);
#6046=EDGE_CURVE('',#4879,#4881,#2380,.T.);
#6047=EDGE_CURVE('',#4882,#4880,#4197,.T.);
#6048=EDGE_CURVE('',#4882,#4883,#2381,.T.);
#6049=EDGE_CURVE('',#4883,#4881,#4198,.T.);
#6050=EDGE_CURVE('',#4884,#4882,#2382,.T.);
#6051=EDGE_CURVE('',#4884,#4885,#2383,.T.);
#6052=EDGE_CURVE('',#4885,#4883,#2384,.T.);
#6053=EDGE_CURVE('',#4886,#4884,#4199,.T.);
#6054=EDGE_CURVE('',#4886,#4887,#2385,.T.);
#6055=EDGE_CURVE('',#4887,#4885,#4200,.T.);
#6056=EDGE_CURVE('',#4888,#4886,#2386,.T.);
#6057=EDGE_CURVE('',#4888,#4889,#2387,.T.);
#6058=EDGE_CURVE('',#4889,#4887,#2388,.T.);
#6059=EDGE_CURVE('',#4874,#4888,#4201,.T.);
#6060=EDGE_CURVE('',#4875,#4889,#4202,.T.);
#6061=EDGE_CURVE('',#4890,#4891,#2389,.T.);
#6062=EDGE_CURVE('',#4892,#4891,#2390,.T.);
#6063=EDGE_CURVE('',#4892,#4893,#2391,.T.);
#6064=EDGE_CURVE('',#4890,#4893,#2392,.T.);
#6065=EDGE_CURVE('',#4894,#4895,#2393,.T.);
#6066=EDGE_CURVE('',#4896,#4895,#2394,.T.);
#6067=EDGE_CURVE('',#4896,#4897,#2395,.T.);
#6068=EDGE_CURVE('',#4894,#4897,#2396,.T.);
#6069=EDGE_CURVE('',#4898,#4899,#2397,.T.);
#6070=EDGE_CURVE('',#4900,#4899,#2398,.T.);
#6071=EDGE_CURVE('',#4900,#4901,#2399,.T.);
#6072=EDGE_CURVE('',#4898,#4901,#2400,.T.);
#6073=EDGE_CURVE('',#4902,#4903,#2401,.T.);
#6074=EDGE_CURVE('',#4904,#4903,#2402,.T.);
#6075=EDGE_CURVE('',#4904,#4905,#2403,.T.);
#6076=EDGE_CURVE('',#4902,#4905,#2404,.T.);
#6077=EDGE_CURVE('',#4906,#4907,#2405,.T.);
#6078=EDGE_CURVE('',#4908,#4907,#2406,.T.);
#6079=EDGE_CURVE('',#4908,#4909,#2407,.T.);
#6080=EDGE_CURVE('',#4906,#4909,#2408,.T.);
#6081=EDGE_CURVE('',#4863,#4908,#4203,.T.);
#6082=EDGE_CURVE('',#4909,#4865,#4204,.T.);
#6083=EDGE_CURVE('',#4907,#4904,#4205,.T.);
#6084=EDGE_CURVE('',#4905,#4906,#4206,.T.);
#6085=EDGE_CURVE('',#4903,#4900,#4207,.T.);
#6086=EDGE_CURVE('',#4901,#4902,#4208,.T.);
#6087=EDGE_CURVE('',#4899,#4892,#4209,.T.);
#6088=EDGE_CURVE('',#4893,#4898,#4210,.T.);
#6089=EDGE_CURVE('',#4891,#4896,#4211,.T.);
#6090=EDGE_CURVE('',#4897,#4890,#4212,.T.);
#6091=EDGE_CURVE('',#4895,#4870,#4213,.T.);
#6092=EDGE_CURVE('',#4872,#4894,#4214,.T.);
#6093=EDGE_CURVE('',#4910,#4910,#4215,.T.);
#6094=EDGE_CURVE('',#4910,#4911,#4216,.T.);
#6095=EDGE_CURVE('',#4911,#4911,#4217,.T.);
#6096=EDGE_CURVE('',#4912,#4913,#4218,.T.);
#6097=EDGE_CURVE('',#4913,#4912,#4219,.T.);
#6098=EDGE_CURVE('',#4913,#4914,#4220,.T.);
#6099=EDGE_CURVE('',#4914,#4914,#4221,.T.);
#6100=EDGE_CURVE('',#4915,#4915,#4222,.T.);
#6101=EDGE_CURVE('',#4915,#4916,#4223,.T.);
#6102=EDGE_CURVE('',#4916,#4916,#4224,.T.);
#6103=EDGE_CURVE('',#4917,#4918,#4225,.T.);
#6104=EDGE_CURVE('',#4918,#4917,#4226,.T.);
#6105=EDGE_CURVE('',#4918,#4919,#4227,.T.);
#6106=EDGE_CURVE('',#4919,#4919,#4228,.T.);
#6107=EDGE_CURVE('',#4912,#4910,#2409,.T.);
#6108=EDGE_CURVE('',#4920,#4920,#4229,.T.);
#6109=EDGE_CURVE('',#4920,#4921,#2410,.T.);
#6110=EDGE_CURVE('',#4921,#4921,#4230,.T.);
#6111=EDGE_CURVE('',#4917,#4915,#2411,.T.);
#6112=EDGE_CURVE('',#4922,#4923,#4231,.T.);
#6113=EDGE_CURVE('',#4923,#4924,#2412,.T.);
#6114=EDGE_CURVE('',#4924,#4925,#4232,.T.);
#6115=EDGE_CURVE('',#4922,#4925,#2413,.T.);
#6116=EDGE_CURVE('',#4926,#4927,#4233,.T.);
#6117=EDGE_CURVE('',#4928,#4926,#2414,.T.);
#6118=EDGE_CURVE('',#4929,#4928,#4234,.T.);
#6119=EDGE_CURVE('',#4929,#4927,#2415,.T.);
#6120=EDGE_CURVE('',#4923,#4928,#2416,.T.);
#6121=EDGE_CURVE('',#4924,#4926,#2417,.T.);
#6122=EDGE_CURVE('',#4922,#4929,#2418,.T.);
#6123=EDGE_CURVE('',#4925,#4927,#2419,.T.);
#6124=EDGE_CURVE('',#4930,#4930,#4235,.T.);
#6125=EDGE_CURVE('',#4930,#4931,#2420,.T.);
#6126=EDGE_CURVE('',#4931,#4931,#4236,.T.);
#6127=EDGE_CURVE('',#4932,#4932,#4237,.T.);
#6128=EDGE_CURVE('',#4932,#4933,#4238,.T.);
#6129=EDGE_CURVE('',#4933,#4933,#4239,.T.);
#6130=EDGE_CURVE('',#4934,#4935,#4240,.T.);
#6131=EDGE_CURVE('',#4935,#4934,#4241,.T.);
#6132=EDGE_CURVE('',#4935,#4936,#4242,.T.);
#6133=EDGE_CURVE('',#4936,#4936,#4243,.T.);
#6134=EDGE_CURVE('',#4937,#4937,#4244,.T.);
#6135=EDGE_CURVE('',#4937,#4938,#4245,.T.);
#6136=EDGE_CURVE('',#4938,#4938,#4246,.T.);
#6137=EDGE_CURVE('',#4939,#4940,#4247,.T.);
#6138=EDGE_CURVE('',#4940,#4939,#4248,.T.);
#6139=EDGE_CURVE('',#4940,#4941,#4249,.T.);
#6140=EDGE_CURVE('',#4941,#4941,#4250,.T.);
#6141=EDGE_CURVE('',#4934,#4932,#2421,.T.);
#6142=EDGE_CURVE('',#4942,#4942,#4251,.T.);
#6143=EDGE_CURVE('',#4942,#4943,#2422,.T.);
#6144=EDGE_CURVE('',#4943,#4943,#4252,.T.);
#6145=EDGE_CURVE('',#4939,#4937,#2423,.T.);
#6146=EDGE_CURVE('',#4944,#4944,#4253,.T.);
#6147=EDGE_CURVE('',#4944,#4945,#4254,.T.);
#6148=EDGE_CURVE('',#4946,#4945,#4255,.T.);
#6149=EDGE_CURVE('',#4945,#4946,#4256,.T.);
#6150=EDGE_CURVE('',#4947,#4947,#4257,.T.);
#6151=EDGE_CURVE('',#4947,#4946,#2424,.T.);
#6152=EDGE_CURVE('',#4948,#4948,#4258,.T.);
#6153=EDGE_CURVE('',#4948,#4949,#2425,.T.);
#6154=EDGE_CURVE('',#4949,#4949,#4259,.T.);
#6155=EDGE_CURVE('',#4950,#4950,#4260,.T.);
#6156=EDGE_CURVE('',#4950,#4951,#2426,.T.);
#6157=EDGE_CURVE('',#4951,#4951,#4261,.T.);
#6158=EDGE_CURVE('',#4952,#4952,#4262,.T.);
#6159=EDGE_CURVE('',#4952,#4953,#2427,.T.);
#6160=EDGE_CURVE('',#4953,#4953,#4263,.T.);
#6161=EDGE_CURVE('',#4954,#4954,#4264,.T.);
#6162=EDGE_CURVE('',#4954,#4955,#2428,.T.);
#6163=EDGE_CURVE('',#4955,#4955,#4265,.T.);
#6164=EDGE_CURVE('',#4956,#4956,#4266,.T.);
#6165=EDGE_CURVE('',#4956,#4957,#2429,.T.);
#6166=EDGE_CURVE('',#4957,#4957,#4267,.T.);
#6167=EDGE_CURVE('',#4958,#4958,#4268,.T.);
#6168=EDGE_CURVE('',#4958,#4959,#2430,.T.);
#6169=EDGE_CURVE('',#4960,#4959,#4269,.T.);
#6170=EDGE_CURVE('',#4960,#4961,#2431,.T.);
#6171=EDGE_CURVE('',#4962,#4961,#4270,.T.);
#6172=EDGE_CURVE('',#4962,#4963,#2432,.T.);
#6173=EDGE_CURVE('',#4964,#4963,#4271,.T.);
#6174=EDGE_CURVE('',#4964,#4965,#2433,.T.);
#6175=EDGE_CURVE('',#4966,#4965,#4272,.T.);
#6176=EDGE_CURVE('',#4966,#4967,#2434,.T.);
#6177=EDGE_CURVE('',#4959,#4967,#4273,.T.);
#6178=EDGE_CURVE('',#4968,#4969,#4274,.T.);
#6179=EDGE_CURVE('',#4968,#4970,#142,.T.);
#6180=EDGE_CURVE('',#4971,#4970,#4275,.T.);
#6181=EDGE_CURVE('',#4969,#4971,#143,.T.);
#6182=EDGE_CURVE('',#4972,#4973,#4276,.T.);
#6183=EDGE_CURVE('',#4973,#4974,#2435,.T.);
#6184=EDGE_CURVE('',#4974,#4975,#4277,.T.);
#6185=EDGE_CURVE('',#4972,#4975,#2436,.T.);
#6186=EDGE_CURVE('',#4976,#4977,#4278,.T.);
#6187=EDGE_CURVE('',#4976,#4978,#2437,.T.);
#6188=EDGE_CURVE('',#4978,#4979,#4279,.T.);
#6189=EDGE_CURVE('',#4979,#4980,#4280,.T.);
#6190=EDGE_CURVE('',#4980,#4977,#2438,.T.);
#6191=EDGE_CURVE('',#4981,#4981,#4281,.T.);
#6192=EDGE_CURVE('',#4981,#4982,#2439,.T.);
#6193=EDGE_CURVE('',#4982,#4983,#4282,.T.);
#6194=EDGE_CURVE('',#4983,#4984,#2440,.T.);
#6195=EDGE_CURVE('',#4984,#4985,#4283,.T.);
#6196=EDGE_CURVE('',#4985,#4986,#2441,.T.);
#6197=EDGE_CURVE('',#4986,#4987,#4284,.T.);
#6198=EDGE_CURVE('',#4987,#4988,#2442,.T.);
#6199=EDGE_CURVE('',#4988,#4989,#4285,.T.);
#6200=EDGE_CURVE('',#4989,#4990,#2443,.T.);
#6201=EDGE_CURVE('',#4990,#4982,#4286,.T.);
#6202=EDGE_CURVE('',#4991,#4980,#2444,.T.);
#6203=EDGE_CURVE('',#4992,#4991,#2445,.T.);
#6204=EDGE_CURVE('',#4993,#4992,#4287,.T.);
#6205=EDGE_CURVE('',#4994,#4993,#2446,.T.);
#6206=EDGE_CURVE('',#4995,#4994,#4288,.T.);
#6207=EDGE_CURVE('',#4996,#4995,#2447,.T.);
#6208=EDGE_CURVE('',#4997,#4996,#2448,.T.);
#6209=EDGE_CURVE('',#4998,#4997,#2449,.T.);
#6210=EDGE_CURVE('',#4998,#4977,#2450,.T.);
#6211=EDGE_CURVE('',#4999,#5000,#2451,.T.);
#6212=EDGE_CURVE('',#4994,#4999,#2452,.T.);
#6213=EDGE_CURVE('',#4993,#5000,#2453,.T.);
#6214=EDGE_CURVE('',#5001,#5002,#2454,.T.);
#6215=EDGE_CURVE('',#5003,#5001,#2455,.T.);
#6216=EDGE_CURVE('',#5004,#5003,#2456,.T.);
#6217=EDGE_CURVE('',#5002,#5004,#2457,.T.);
#6218=EDGE_CURVE('',#4986,#4983,#2458,.T.);
#6219=EDGE_CURVE('',#4990,#4987,#2459,.T.);
#6220=EDGE_CURVE('',#4998,#5005,#4289,.T.);
#6221=EDGE_CURVE('',#4976,#5005,#2460,.T.);
#6222=EDGE_CURVE('',#5006,#4974,#2461,.T.);
#6223=EDGE_CURVE('',#5007,#5006,#4290,.T.);
#6224=EDGE_CURVE('',#4975,#5007,#2462,.T.);
#6225=EDGE_CURVE('',#4997,#5008,#4291,.T.);
#6226=EDGE_CURVE('',#5008,#5009,#4292,.T.);
#6227=EDGE_CURVE('',#5009,#5005,#2463,.T.);
#6228=EDGE_CURVE('',#4991,#4979,#2464,.T.);
#6229=EDGE_CURVE('',#5008,#5010,#2465,.T.);
#6230=EDGE_CURVE('',#5011,#5010,#2466,.T.);
#6231=EDGE_CURVE('',#4979,#5011,#2467,.T.);
#6232=EDGE_CURVE('',#4978,#5009,#2468,.T.);
#6233=EDGE_CURVE('',#4996,#5008,#2469,.T.);
#6234=EDGE_CURVE('',#5012,#5011,#2470,.T.);
#6235=EDGE_CURVE('',#4992,#5012,#2471,.T.);
#6236=EDGE_CURVE('',#5000,#5012,#4293,.T.);
#6237=EDGE_CURVE('',#5013,#4999,#4294,.T.);
#6238=EDGE_CURVE('',#4995,#5013,#2472,.T.);
#6239=EDGE_CURVE('',#5010,#5013,#2473,.T.);
#6240=EDGE_CURVE('',#4968,#5006,#2474,.T.);
#6241=EDGE_CURVE('',#4969,#5007,#2475,.T.);
#6242=EDGE_CURVE('',#4973,#4968,#2476,.T.);
#6243=EDGE_CURVE('',#4969,#4972,#2477,.T.);
#6244=EDGE_CURVE('',#5014,#5015,#4295,.T.);
#6245=EDGE_CURVE('',#5015,#4971,#2478,.T.);
#6246=EDGE_CURVE('',#4970,#5014,#2479,.T.);
#6247=EDGE_CURVE('',#5014,#4973,#144,.T.);
#6248=EDGE_CURVE('',#5015,#4972,#145,.T.);
#6249=EDGE_CURVE('',#4960,#4963,#2480,.T.);
#6250=EDGE_CURVE('',#4964,#4967,#2481,.T.);
#6251=EDGE_CURVE('',#4965,#4966,#2482,.T.);
#6252=EDGE_CURVE('',#4961,#4962,#2483,.T.);
#6253=EDGE_CURVE('',#4989,#4988,#2484,.T.);
#6254=EDGE_CURVE('',#4985,#4984,#2485,.T.);
#6255=EDGE_CURVE('',#5016,#5001,#2486,.T.);
#6256=EDGE_CURVE('',#5017,#5016,#2487,.T.);
#6257=EDGE_CURVE('',#5017,#5003,#2488,.T.);
#6258=EDGE_CURVE('',#5018,#5002,#2489,.T.);
#6259=EDGE_CURVE('',#5016,#5018,#2490,.T.);
#6260=EDGE_CURVE('',#5019,#5004,#2491,.T.);
#6261=EDGE_CURVE('',#5018,#5019,#2492,.T.);
#6262=EDGE_CURVE('',#5019,#5017,#2493,.T.);
#6263=EDGE_CURVE('',#5020,#5021,#4296,.T.);
#6264=EDGE_CURVE('',#5021,#5022,#2494,.T.);
#6265=EDGE_CURVE('',#5023,#5022,#4297,.T.);
#6266=EDGE_CURVE('',#5020,#5023,#2495,.T.);
#6267=EDGE_CURVE('',#5024,#5025,#4298,.T.);
#6268=EDGE_CURVE('',#5024,#5026,#2496,.T.);
#6269=EDGE_CURVE('',#5026,#5027,#4299,.T.);
#6270=EDGE_CURVE('',#5025,#5027,#2497,.T.);
#6271=EDGE_CURVE('',#5025,#5028,#2498,.T.);
#6272=EDGE_CURVE('',#5028,#5029,#4300,.T.);
#6273=EDGE_CURVE('',#5029,#5024,#2499,.T.);
#6274=EDGE_CURVE('',#5021,#5030,#2500,.T.);
#6275=EDGE_CURVE('',#5031,#5020,#2501,.T.);
#6276=EDGE_CURVE('',#5030,#5031,#4301,.T.);
#6277=EDGE_CURVE('',#5032,#5026,#2502,.T.);
#6278=EDGE_CURVE('',#5033,#5032,#4302,.T.);
#6279=EDGE_CURVE('',#5027,#5033,#2503,.T.);
#6280=EDGE_CURVE('',#5022,#5034,#2504,.T.);
#6281=EDGE_CURVE('',#5034,#5035,#4303,.T.);
#6282=EDGE_CURVE('',#5035,#5023,#2505,.T.);
#6283=EDGE_CURVE('',#5028,#5033,#2506,.T.);
#6284=EDGE_CURVE('',#5029,#5032,#2507,.T.);
#6285=EDGE_CURVE('',#5030,#5034,#2508,.T.);
#6286=EDGE_CURVE('',#5031,#5035,#2509,.T.);
#6287=EDGE_CURVE('',#5036,#5037,#4304,.T.);
#6288=EDGE_CURVE('',#5037,#5038,#2510,.T.);
#6289=EDGE_CURVE('',#5039,#5038,#4305,.T.);
#6290=EDGE_CURVE('',#5036,#5039,#2511,.T.);
#6291=EDGE_CURVE('',#5040,#5041,#4306,.T.);
#6292=EDGE_CURVE('',#5040,#5042,#2512,.T.);
#6293=EDGE_CURVE('',#5042,#5043,#4307,.T.);
#6294=EDGE_CURVE('',#5041,#5043,#2513,.T.);
#6295=EDGE_CURVE('',#5041,#5044,#2514,.T.);
#6296=EDGE_CURVE('',#5044,#5045,#2515,.T.);
#6297=EDGE_CURVE('',#5045,#5046,#2516,.T.);
#6298=EDGE_CURVE('',#5046,#5047,#4308,.T.);
#6299=EDGE_CURVE('',#5047,#5040,#2517,.T.);
#6300=EDGE_CURVE('',#5037,#5048,#2518,.T.);
#6301=EDGE_CURVE('',#5049,#5036,#2519,.T.);
#6302=EDGE_CURVE('',#5050,#5049,#4309,.T.);
#6303=EDGE_CURVE('',#5051,#5050,#2520,.T.);
#6304=EDGE_CURVE('',#5048,#5051,#2521,.T.);
#6305=EDGE_CURVE('',#5052,#5042,#2522,.T.);
#6306=EDGE_CURVE('',#5053,#5052,#4310,.T.);
#6307=EDGE_CURVE('',#5054,#5053,#2523,.T.);
#6308=EDGE_CURVE('',#5055,#5054,#2524,.T.);
#6309=EDGE_CURVE('',#5043,#5055,#2525,.T.);
#6310=EDGE_CURVE('',#5038,#5056,#2526,.T.);
#6311=EDGE_CURVE('',#5056,#5057,#2527,.T.);
#6312=EDGE_CURVE('',#5057,#5058,#2528,.T.);
#6313=EDGE_CURVE('',#5058,#5059,#4311,.T.);
#6314=EDGE_CURVE('',#5059,#5039,#2529,.T.);
#6315=EDGE_CURVE('',#5044,#5055,#2530,.T.);
#6316=EDGE_CURVE('',#5045,#5054,#2531,.T.);
#6317=EDGE_CURVE('',#5046,#5053,#2532,.T.);
#6318=EDGE_CURVE('',#5047,#5052,#2533,.T.);
#6319=EDGE_CURVE('',#5048,#5056,#2534,.T.);
#6320=EDGE_CURVE('',#5051,#5057,#2535,.T.);
#6321=EDGE_CURVE('',#5050,#5058,#2536,.T.);
#6322=EDGE_CURVE('',#5049,#5059,#2537,.T.);
#6323=EDGE_CURVE('',#5060,#5061,#4312,.T.);
#6324=EDGE_CURVE('',#5061,#5062,#2538,.T.);
#6325=EDGE_CURVE('',#5063,#5062,#4313,.T.);
#6326=EDGE_CURVE('',#5060,#5063,#2539,.T.);
#6327=EDGE_CURVE('',#5064,#5065,#2540,.T.);
#6328=EDGE_CURVE('',#5065,#5066,#2541,.T.);
#6329=EDGE_CURVE('',#5066,#5067,#2542,.T.);
#6330=EDGE_CURVE('',#5067,#5068,#2543,.T.);
#6331=EDGE_CURVE('',#5068,#5069,#2544,.T.);
#6332=EDGE_CURVE('',#5069,#5070,#4314,.T.);
#6333=EDGE_CURVE('',#5070,#5071,#2545,.T.);
#6334=EDGE_CURVE('',#5071,#5072,#4315,.T.);
#6335=EDGE_CURVE('',#5072,#5073,#2546,.T.);
#6336=EDGE_CURVE('',#5073,#5074,#4316,.T.);
#6337=EDGE_CURVE('',#5074,#5075,#2547,.T.);
#6338=EDGE_CURVE('',#5075,#5076,#4317,.T.);
#6339=EDGE_CURVE('',#5076,#5077,#2548,.T.);
#6340=EDGE_CURVE('',#5077,#5078,#4318,.T.);
#6341=EDGE_CURVE('',#5078,#5079,#2549,.T.);
#6342=EDGE_CURVE('',#5079,#5080,#4319,.T.);
#6343=EDGE_CURVE('',#5080,#5081,#2550,.T.);
#6344=EDGE_CURVE('',#5081,#5082,#4320,.T.);
#6345=EDGE_CURVE('',#5082,#5083,#2551,.T.);
#6346=EDGE_CURVE('',#5083,#5084,#4321,.T.);
#6347=EDGE_CURVE('',#5084,#5085,#2552,.T.);
#6348=EDGE_CURVE('',#5085,#5086,#4322,.T.);
#6349=EDGE_CURVE('',#5086,#5087,#2553,.T.);
#6350=EDGE_CURVE('',#5087,#5088,#4323,.T.);
#6351=EDGE_CURVE('',#5088,#5089,#2554,.T.);
#6352=EDGE_CURVE('',#5089,#5090,#4324,.T.);
#6353=EDGE_CURVE('',#5090,#5091,#2555,.T.);
#6354=EDGE_CURVE('',#5091,#5092,#2556,.T.);
#6355=EDGE_CURVE('',#5092,#5093,#2557,.T.);
#6356=EDGE_CURVE('',#5093,#5094,#2558,.T.);
#6357=EDGE_CURVE('',#5094,#5095,#2559,.T.);
#6358=EDGE_CURVE('',#5095,#5096,#2560,.T.);
#6359=EDGE_CURVE('',#5096,#5097,#2561,.T.);
#6360=EDGE_CURVE('',#5097,#5098,#2562,.T.);
#6361=EDGE_CURVE('',#5098,#5099,#4325,.T.);
#6362=EDGE_CURVE('',#5099,#5100,#2563,.T.);
#6363=EDGE_CURVE('',#5100,#5101,#4326,.T.);
#6364=EDGE_CURVE('',#5101,#5102,#2564,.T.);
#6365=EDGE_CURVE('',#5102,#5103,#4327,.T.);
#6366=EDGE_CURVE('',#5103,#5104,#2565,.T.);
#6367=EDGE_CURVE('',#5104,#5105,#4328,.T.);
#6368=EDGE_CURVE('',#5105,#5106,#2566,.T.);
#6369=EDGE_CURVE('',#5106,#5107,#4329,.T.);
#6370=EDGE_CURVE('',#5107,#5108,#2567,.T.);
#6371=EDGE_CURVE('',#5108,#5109,#4330,.T.);
#6372=EDGE_CURVE('',#5109,#5110,#2568,.T.);
#6373=EDGE_CURVE('',#5110,#5111,#4331,.T.);
#6374=EDGE_CURVE('',#5111,#5112,#2569,.T.);
#6375=EDGE_CURVE('',#5112,#5113,#4332,.T.);
#6376=EDGE_CURVE('',#5113,#5114,#2570,.T.);
#6377=EDGE_CURVE('',#5114,#5115,#4333,.T.);
#6378=EDGE_CURVE('',#5115,#5116,#2571,.T.);
#6379=EDGE_CURVE('',#5116,#5117,#4334,.T.);
#6380=EDGE_CURVE('',#5117,#5118,#2572,.T.);
#6381=EDGE_CURVE('',#5118,#5119,#4335,.T.);
#6382=EDGE_CURVE('',#5119,#5120,#2573,.T.);
#6383=EDGE_CURVE('',#5120,#5121,#2574,.T.);
#6384=EDGE_CURVE('',#5121,#5122,#2575,.T.);
#6385=EDGE_CURVE('',#5122,#5123,#2576,.T.);
#6386=EDGE_CURVE('',#5123,#5124,#2577,.T.);
#6387=EDGE_CURVE('',#5124,#5125,#2578,.T.);
#6388=EDGE_CURVE('',#5125,#5126,#2579,.T.);
#6389=EDGE_CURVE('',#5126,#5127,#2580,.T.);
#6390=EDGE_CURVE('',#5127,#5128,#4336,.T.);
#6391=EDGE_CURVE('',#5128,#5129,#2581,.T.);
#6392=EDGE_CURVE('',#5129,#5130,#4337,.T.);
#6393=EDGE_CURVE('',#5130,#5131,#2582,.T.);
#6394=EDGE_CURVE('',#5131,#5132,#4338,.T.);
#6395=EDGE_CURVE('',#5132,#5133,#2583,.T.);
#6396=EDGE_CURVE('',#5133,#5134,#4339,.T.);
#6397=EDGE_CURVE('',#5134,#5135,#2584,.T.);
#6398=EDGE_CURVE('',#5135,#5136,#4340,.T.);
#6399=EDGE_CURVE('',#5136,#5137,#2585,.T.);
#6400=EDGE_CURVE('',#5137,#5138,#4341,.T.);
#6401=EDGE_CURVE('',#5138,#5139,#2586,.T.);
#6402=EDGE_CURVE('',#5139,#5140,#4342,.T.);
#6403=EDGE_CURVE('',#5140,#5141,#2587,.T.);
#6404=EDGE_CURVE('',#5141,#5142,#4343,.T.);
#6405=EDGE_CURVE('',#5142,#5143,#2588,.T.);
#6406=EDGE_CURVE('',#5143,#5144,#4344,.T.);
#6407=EDGE_CURVE('',#5144,#5145,#2589,.T.);
#6408=EDGE_CURVE('',#5145,#5146,#4345,.T.);
#6409=EDGE_CURVE('',#5146,#5147,#2590,.T.);
#6410=EDGE_CURVE('',#5147,#5148,#4346,.T.);
#6411=EDGE_CURVE('',#5148,#5149,#2591,.T.);
#6412=EDGE_CURVE('',#5149,#5150,#2592,.T.);
#6413=EDGE_CURVE('',#5150,#5151,#2593,.T.);
#6414=EDGE_CURVE('',#5151,#5152,#2594,.T.);
#6415=EDGE_CURVE('',#5152,#5153,#2595,.T.);
#6416=EDGE_CURVE('',#5153,#5154,#2596,.T.);
#6417=EDGE_CURVE('',#5154,#5155,#2597,.T.);
#6418=EDGE_CURVE('',#5155,#5156,#2598,.T.);
#6419=EDGE_CURVE('',#5156,#5157,#4347,.T.);
#6420=EDGE_CURVE('',#5157,#5158,#2599,.T.);
#6421=EDGE_CURVE('',#5158,#5159,#4348,.T.);
#6422=EDGE_CURVE('',#5159,#5160,#2600,.T.);
#6423=EDGE_CURVE('',#5160,#5161,#4349,.T.);
#6424=EDGE_CURVE('',#5161,#5162,#2601,.T.);
#6425=EDGE_CURVE('',#5162,#5163,#4350,.T.);
#6426=EDGE_CURVE('',#5163,#5164,#2602,.T.);
#6427=EDGE_CURVE('',#5164,#5165,#4351,.T.);
#6428=EDGE_CURVE('',#5165,#5166,#2603,.T.);
#6429=EDGE_CURVE('',#5166,#5167,#4352,.T.);
#6430=EDGE_CURVE('',#5167,#5168,#2604,.T.);
#6431=EDGE_CURVE('',#5168,#5169,#4353,.T.);
#6432=EDGE_CURVE('',#5169,#5170,#2605,.T.);
#6433=EDGE_CURVE('',#5170,#5171,#4354,.T.);
#6434=EDGE_CURVE('',#5171,#5172,#2606,.T.);
#6435=EDGE_CURVE('',#5172,#5173,#4355,.T.);
#6436=EDGE_CURVE('',#5173,#5174,#2607,.T.);
#6437=EDGE_CURVE('',#5174,#5175,#4356,.T.);
#6438=EDGE_CURVE('',#5175,#5176,#2608,.T.);
#6439=EDGE_CURVE('',#5176,#5177,#4357,.T.);
#6440=EDGE_CURVE('',#5177,#5178,#2609,.T.);
#6441=EDGE_CURVE('',#5178,#5179,#2610,.T.);
#6442=EDGE_CURVE('',#5179,#5064,#2611,.T.);
#6443=EDGE_CURVE('',#5180,#5181,#2612,.T.);
#6444=EDGE_CURVE('',#5182,#5180,#4358,.T.);
#6445=EDGE_CURVE('',#5183,#5182,#2613,.T.);
#6446=EDGE_CURVE('',#5184,#5183,#4359,.T.);
#6447=EDGE_CURVE('',#5185,#5184,#2614,.T.);
#6448=EDGE_CURVE('',#5186,#5185,#4360,.T.);
#6449=EDGE_CURVE('',#5187,#5186,#2615,.T.);
#6450=EDGE_CURVE('',#5181,#5187,#4361,.T.);
#6451=EDGE_CURVE('',#5188,#5189,#2616,.T.);
#6452=EDGE_CURVE('',#5190,#5188,#4362,.T.);
#6453=EDGE_CURVE('',#5191,#5190,#2617,.T.);
#6454=EDGE_CURVE('',#5192,#5191,#4363,.T.);
#6455=EDGE_CURVE('',#5193,#5192,#2618,.T.);
#6456=EDGE_CURVE('',#5194,#5193,#4364,.T.);
#6457=EDGE_CURVE('',#5195,#5194,#2619,.T.);
#6458=EDGE_CURVE('',#5196,#5195,#4365,.T.);
#6459=EDGE_CURVE('',#5197,#5196,#2620,.T.);
#6460=EDGE_CURVE('',#5198,#5197,#4366,.T.);
#6461=EDGE_CURVE('',#5199,#5198,#2621,.T.);
#6462=EDGE_CURVE('',#5200,#5199,#4367,.T.);
#6463=EDGE_CURVE('',#5061,#5200,#2622,.T.);
#6464=EDGE_CURVE('',#5201,#5060,#2623,.T.);
#6465=EDGE_CURVE('',#5189,#5201,#4368,.T.);
#6466=EDGE_CURVE('',#5202,#5203,#2624,.T.);
#6467=EDGE_CURVE('',#5204,#5202,#4369,.T.);
#6468=EDGE_CURVE('',#5205,#5204,#2625,.T.);
#6469=EDGE_CURVE('',#5206,#5205,#4370,.T.);
#6470=EDGE_CURVE('',#5207,#5206,#2626,.T.);
#6471=EDGE_CURVE('',#5208,#5207,#4371,.T.);
#6472=EDGE_CURVE('',#5209,#5208,#2627,.T.);
#6473=EDGE_CURVE('',#5203,#5209,#4372,.T.);
#6474=EDGE_CURVE('',#5210,#5211,#2628,.T.);
#6475=EDGE_CURVE('',#5212,#5210,#4373,.T.);
#6476=EDGE_CURVE('',#5213,#5212,#2629,.T.);
#6477=EDGE_CURVE('',#5214,#5213,#4374,.T.);
#6478=EDGE_CURVE('',#5215,#5214,#2630,.T.);
#6479=EDGE_CURVE('',#5216,#5215,#4375,.T.);
#6480=EDGE_CURVE('',#5217,#5216,#2631,.T.);
#6481=EDGE_CURVE('',#5211,#5217,#4376,.T.);
#6482=EDGE_CURVE('',#5218,#5219,#2632,.T.);
#6483=EDGE_CURVE('',#5220,#5218,#4377,.T.);
#6484=EDGE_CURVE('',#5221,#5220,#2633,.T.);
#6485=EDGE_CURVE('',#5222,#5221,#4378,.T.);
#6486=EDGE_CURVE('',#5223,#5222,#2634,.T.);
#6487=EDGE_CURVE('',#5224,#5223,#4379,.T.);
#6488=EDGE_CURVE('',#5225,#5224,#2635,.T.);
#6489=EDGE_CURVE('',#5219,#5225,#4380,.T.);
#6490=EDGE_CURVE('',#5226,#5227,#2636,.T.);
#6491=EDGE_CURVE('',#5228,#5226,#2637,.T.);
#6492=EDGE_CURVE('',#5229,#5228,#2638,.T.);
#6493=EDGE_CURVE('',#5230,#5229,#2639,.T.);
#6494=EDGE_CURVE('',#5231,#5230,#4381,.T.);
#6495=EDGE_CURVE('',#5232,#5231,#2640,.T.);
#6496=EDGE_CURVE('',#5233,#5232,#4382,.T.);
#6497=EDGE_CURVE('',#5234,#5233,#2641,.T.);
#6498=EDGE_CURVE('',#5235,#5234,#4383,.T.);
#6499=EDGE_CURVE('',#5236,#5235,#2642,.T.);
#6500=EDGE_CURVE('',#5237,#5236,#4384,.T.);
#6501=EDGE_CURVE('',#5238,#5237,#2643,.T.);
#6502=EDGE_CURVE('',#5239,#5238,#4385,.T.);
#6503=EDGE_CURVE('',#5240,#5239,#2644,.T.);
#6504=EDGE_CURVE('',#5241,#5240,#4386,.T.);
#6505=EDGE_CURVE('',#5242,#5241,#2645,.T.);
#6506=EDGE_CURVE('',#5243,#5242,#4387,.T.);
#6507=EDGE_CURVE('',#5244,#5243,#2646,.T.);
#6508=EDGE_CURVE('',#5245,#5244,#4388,.T.);
#6509=EDGE_CURVE('',#5246,#5245,#2647,.T.);
#6510=EDGE_CURVE('',#5247,#5246,#4389,.T.);
#6511=EDGE_CURVE('',#5248,#5247,#2648,.T.);
#6512=EDGE_CURVE('',#5249,#5248,#4390,.T.);
#6513=EDGE_CURVE('',#5250,#5249,#2649,.T.);
#6514=EDGE_CURVE('',#5251,#5250,#4391,.T.);
#6515=EDGE_CURVE('',#5252,#5251,#2650,.T.);
#6516=EDGE_CURVE('',#5253,#5252,#2651,.T.);
#6517=EDGE_CURVE('',#5254,#5253,#2652,.T.);
#6518=EDGE_CURVE('',#5255,#5254,#2653,.T.);
#6519=EDGE_CURVE('',#5256,#5255,#2654,.T.);
#6520=EDGE_CURVE('',#5257,#5256,#2655,.T.);
#6521=EDGE_CURVE('',#5258,#5257,#2656,.T.);
#6522=EDGE_CURVE('',#5259,#5258,#2657,.T.);
#6523=EDGE_CURVE('',#5260,#5259,#4392,.T.);
#6524=EDGE_CURVE('',#5261,#5260,#2658,.T.);
#6525=EDGE_CURVE('',#5262,#5261,#4393,.T.);
#6526=EDGE_CURVE('',#5263,#5262,#2659,.T.);
#6527=EDGE_CURVE('',#5264,#5263,#4394,.T.);
#6528=EDGE_CURVE('',#5265,#5264,#2660,.T.);
#6529=EDGE_CURVE('',#5266,#5265,#4395,.T.);
#6530=EDGE_CURVE('',#5267,#5266,#2661,.T.);
#6531=EDGE_CURVE('',#5268,#5267,#4396,.T.);
#6532=EDGE_CURVE('',#5269,#5268,#2662,.T.);
#6533=EDGE_CURVE('',#5270,#5269,#4397,.T.);
#6534=EDGE_CURVE('',#5271,#5270,#2663,.T.);
#6535=EDGE_CURVE('',#5272,#5271,#4398,.T.);
#6536=EDGE_CURVE('',#5273,#5272,#2664,.T.);
#6537=EDGE_CURVE('',#5274,#5273,#4399,.T.);
#6538=EDGE_CURVE('',#5275,#5274,#2665,.T.);
#6539=EDGE_CURVE('',#5276,#5275,#4400,.T.);
#6540=EDGE_CURVE('',#5277,#5276,#2666,.T.);
#6541=EDGE_CURVE('',#5278,#5277,#4401,.T.);
#6542=EDGE_CURVE('',#5279,#5278,#2667,.T.);
#6543=EDGE_CURVE('',#5280,#5279,#4402,.T.);
#6544=EDGE_CURVE('',#5281,#5280,#2668,.T.);
#6545=EDGE_CURVE('',#5282,#5281,#2669,.T.);
#6546=EDGE_CURVE('',#5283,#5282,#2670,.T.);
#6547=EDGE_CURVE('',#5284,#5283,#2671,.T.);
#6548=EDGE_CURVE('',#5285,#5284,#2672,.T.);
#6549=EDGE_CURVE('',#5286,#5285,#2673,.T.);
#6550=EDGE_CURVE('',#5287,#5286,#2674,.T.);
#6551=EDGE_CURVE('',#5288,#5287,#2675,.T.);
#6552=EDGE_CURVE('',#5289,#5288,#4403,.T.);
#6553=EDGE_CURVE('',#5290,#5289,#2676,.T.);
#6554=EDGE_CURVE('',#5291,#5290,#4404,.T.);
#6555=EDGE_CURVE('',#5292,#5291,#2677,.T.);
#6556=EDGE_CURVE('',#5293,#5292,#4405,.T.);
#6557=EDGE_CURVE('',#5294,#5293,#2678,.T.);
#6558=EDGE_CURVE('',#5295,#5294,#4406,.T.);
#6559=EDGE_CURVE('',#5296,#5295,#2679,.T.);
#6560=EDGE_CURVE('',#5297,#5296,#4407,.T.);
#6561=EDGE_CURVE('',#5298,#5297,#2680,.T.);
#6562=EDGE_CURVE('',#5299,#5298,#4408,.T.);
#6563=EDGE_CURVE('',#5300,#5299,#2681,.T.);
#6564=EDGE_CURVE('',#5301,#5300,#4409,.T.);
#6565=EDGE_CURVE('',#5302,#5301,#2682,.T.);
#6566=EDGE_CURVE('',#5303,#5302,#4410,.T.);
#6567=EDGE_CURVE('',#5304,#5303,#2683,.T.);
#6568=EDGE_CURVE('',#5305,#5304,#4411,.T.);
#6569=EDGE_CURVE('',#5306,#5305,#2684,.T.);
#6570=EDGE_CURVE('',#5307,#5306,#4412,.T.);
#6571=EDGE_CURVE('',#5308,#5307,#2685,.T.);
#6572=EDGE_CURVE('',#5309,#5308,#4413,.T.);
#6573=EDGE_CURVE('',#5310,#5309,#2686,.T.);
#6574=EDGE_CURVE('',#5311,#5310,#2687,.T.);
#6575=EDGE_CURVE('',#5312,#5311,#2688,.T.);
#6576=EDGE_CURVE('',#5313,#5312,#2689,.T.);
#6577=EDGE_CURVE('',#5314,#5313,#2690,.T.);
#6578=EDGE_CURVE('',#5315,#5314,#2691,.T.);
#6579=EDGE_CURVE('',#5316,#5315,#2692,.T.);
#6580=EDGE_CURVE('',#5317,#5316,#2693,.T.);
#6581=EDGE_CURVE('',#5318,#5317,#4414,.T.);
#6582=EDGE_CURVE('',#5319,#5318,#2694,.T.);
#6583=EDGE_CURVE('',#5320,#5319,#4415,.T.);
#6584=EDGE_CURVE('',#5321,#5320,#2695,.T.);
#6585=EDGE_CURVE('',#5322,#5321,#4416,.T.);
#6586=EDGE_CURVE('',#5323,#5322,#2696,.T.);
#6587=EDGE_CURVE('',#5324,#5323,#4417,.T.);
#6588=EDGE_CURVE('',#5325,#5324,#2697,.T.);
#6589=EDGE_CURVE('',#5326,#5325,#4418,.T.);
#6590=EDGE_CURVE('',#5327,#5326,#2698,.T.);
#6591=EDGE_CURVE('',#5328,#5327,#4419,.T.);
#6592=EDGE_CURVE('',#5329,#5328,#2699,.T.);
#6593=EDGE_CURVE('',#5330,#5329,#4420,.T.);
#6594=EDGE_CURVE('',#5331,#5330,#2700,.T.);
#6595=EDGE_CURVE('',#5332,#5331,#4421,.T.);
#6596=EDGE_CURVE('',#5333,#5332,#2701,.T.);
#6597=EDGE_CURVE('',#5334,#5333,#4422,.T.);
#6598=EDGE_CURVE('',#5335,#5334,#2702,.T.);
#6599=EDGE_CURVE('',#5336,#5335,#4423,.T.);
#6600=EDGE_CURVE('',#5337,#5336,#2703,.T.);
#6601=EDGE_CURVE('',#5338,#5337,#4424,.T.);
#6602=EDGE_CURVE('',#5339,#5338,#2704,.T.);
#6603=EDGE_CURVE('',#5340,#5339,#2705,.T.);
#6604=EDGE_CURVE('',#5341,#5340,#2706,.T.);
#6605=EDGE_CURVE('',#5227,#5341,#2707,.T.);
#6606=EDGE_CURVE('',#5342,#5343,#4425,.T.);
#6607=EDGE_CURVE('',#5343,#5344,#2708,.T.);
#6608=EDGE_CURVE('',#5344,#5345,#4426,.T.);
#6609=EDGE_CURVE('',#5345,#5346,#2709,.T.);
#6610=EDGE_CURVE('',#5346,#5347,#4427,.T.);
#6611=EDGE_CURVE('',#5347,#5348,#2710,.T.);
#6612=EDGE_CURVE('',#5348,#5349,#4428,.T.);
#6613=EDGE_CURVE('',#5349,#5342,#2711,.T.);
#6614=EDGE_CURVE('',#5350,#5351,#4429,.T.);
#6615=EDGE_CURVE('',#5351,#5352,#2712,.T.);
#6616=EDGE_CURVE('',#5352,#5353,#4430,.T.);
#6617=EDGE_CURVE('',#5353,#5354,#2713,.T.);
#6618=EDGE_CURVE('',#5354,#5355,#4431,.T.);
#6619=EDGE_CURVE('',#5355,#5356,#2714,.T.);
#6620=EDGE_CURVE('',#5356,#5357,#4432,.T.);
#6621=EDGE_CURVE('',#5357,#5350,#2715,.T.);
#6622=EDGE_CURVE('',#5358,#5359,#4433,.T.);
#6623=EDGE_CURVE('',#5359,#5360,#2716,.T.);
#6624=EDGE_CURVE('',#5360,#5361,#4434,.T.);
#6625=EDGE_CURVE('',#5361,#5362,#2717,.T.);
#6626=EDGE_CURVE('',#5362,#5363,#4435,.T.);
#6627=EDGE_CURVE('',#5363,#5364,#2718,.T.);
#6628=EDGE_CURVE('',#5364,#5365,#4436,.T.);
#6629=EDGE_CURVE('',#5365,#5358,#2719,.T.);
#6630=EDGE_CURVE('',#5366,#5367,#4437,.T.);
#6631=EDGE_CURVE('',#5367,#5368,#2720,.T.);
#6632=EDGE_CURVE('',#5368,#5369,#4438,.T.);
#6633=EDGE_CURVE('',#5369,#5370,#2721,.T.);
#6634=EDGE_CURVE('',#5370,#5371,#4439,.T.);
#6635=EDGE_CURVE('',#5371,#5372,#2722,.T.);
#6636=EDGE_CURVE('',#5372,#5373,#4440,.T.);
#6637=EDGE_CURVE('',#5373,#5366,#2723,.T.);
#6638=EDGE_CURVE('',#5374,#5375,#4441,.T.);
#6639=EDGE_CURVE('',#5375,#5376,#2724,.T.);
#6640=EDGE_CURVE('',#5376,#5377,#4442,.T.);
#6641=EDGE_CURVE('',#5377,#5063,#2725,.T.);
#6642=EDGE_CURVE('',#5062,#5378,#2726,.T.);
#6643=EDGE_CURVE('',#5378,#5379,#4443,.T.);
#6644=EDGE_CURVE('',#5379,#5380,#2727,.T.);
#6645=EDGE_CURVE('',#5380,#5381,#4444,.T.);
#6646=EDGE_CURVE('',#5381,#5382,#2728,.T.);
#6647=EDGE_CURVE('',#5382,#5383,#4445,.T.);
#6648=EDGE_CURVE('',#5383,#5384,#2729,.T.);
#6649=EDGE_CURVE('',#5384,#5385,#4446,.T.);
#6650=EDGE_CURVE('',#5385,#5386,#2730,.T.);
#6651=EDGE_CURVE('',#5386,#5387,#4447,.T.);
#6652=EDGE_CURVE('',#5387,#5374,#2731,.T.);
#6653=EDGE_CURVE('',#5065,#5227,#2732,.T.);
#6654=EDGE_CURVE('',#5064,#5226,#2733,.T.);
#6655=EDGE_CURVE('',#5066,#5341,#2734,.T.);
#6656=EDGE_CURVE('',#5067,#5340,#2735,.T.);
#6657=EDGE_CURVE('',#5068,#5339,#2736,.T.);
#6658=EDGE_CURVE('',#5069,#5338,#2737,.T.);
#6659=EDGE_CURVE('',#5070,#5337,#2738,.T.);
#6660=EDGE_CURVE('',#5071,#5336,#2739,.T.);
#6661=EDGE_CURVE('',#5072,#5335,#2740,.T.);
#6662=EDGE_CURVE('',#5073,#5334,#2741,.T.);
#6663=EDGE_CURVE('',#5074,#5333,#2742,.T.);
#6664=EDGE_CURVE('',#5075,#5332,#2743,.T.);
#6665=EDGE_CURVE('',#5076,#5331,#2744,.T.);
#6666=EDGE_CURVE('',#5077,#5330,#2745,.T.);
#6667=EDGE_CURVE('',#5078,#5329,#2746,.T.);
#6668=EDGE_CURVE('',#5079,#5328,#2747,.T.);
#6669=EDGE_CURVE('',#5080,#5327,#2748,.T.);
#6670=EDGE_CURVE('',#5081,#5326,#2749,.T.);
#6671=EDGE_CURVE('',#5082,#5325,#2750,.T.);
#6672=EDGE_CURVE('',#5083,#5324,#2751,.T.);
#6673=EDGE_CURVE('',#5084,#5323,#2752,.T.);
#6674=EDGE_CURVE('',#5085,#5322,#2753,.T.);
#6675=EDGE_CURVE('',#5086,#5321,#2754,.T.);
#6676=EDGE_CURVE('',#5087,#5320,#2755,.T.);
#6677=EDGE_CURVE('',#5088,#5319,#2756,.T.);
#6678=EDGE_CURVE('',#5089,#5318,#2757,.T.);
#6679=EDGE_CURVE('',#5090,#5317,#2758,.T.);
#6680=EDGE_CURVE('',#5091,#5316,#2759,.T.);
#6681=EDGE_CURVE('',#5092,#5315,#2760,.T.);
#6682=EDGE_CURVE('',#5093,#5314,#2761,.T.);
#6683=EDGE_CURVE('',#5094,#5313,#2762,.T.);
#6684=EDGE_CURVE('',#5095,#5312,#2763,.T.);
#6685=EDGE_CURVE('',#5096,#5311,#2764,.T.);
#6686=EDGE_CURVE('',#5097,#5310,#2765,.T.);
#6687=EDGE_CURVE('',#5098,#5309,#2766,.T.);
#6688=EDGE_CURVE('',#5099,#5308,#2767,.T.);
#6689=EDGE_CURVE('',#5100,#5307,#2768,.T.);
#6690=EDGE_CURVE('',#5101,#5306,#2769,.T.);
#6691=EDGE_CURVE('',#5102,#5305,#2770,.T.);
#6692=EDGE_CURVE('',#5103,#5304,#2771,.T.);
#6693=EDGE_CURVE('',#5104,#5303,#2772,.T.);
#6694=EDGE_CURVE('',#5105,#5302,#2773,.T.);
#6695=EDGE_CURVE('',#5106,#5301,#2774,.T.);
#6696=EDGE_CURVE('',#5107,#5300,#2775,.T.);
#6697=EDGE_CURVE('',#5108,#5299,#2776,.T.);
#6698=EDGE_CURVE('',#5109,#5298,#2777,.T.);
#6699=EDGE_CURVE('',#5110,#5297,#2778,.T.);
#6700=EDGE_CURVE('',#5111,#5296,#2779,.T.);
#6701=EDGE_CURVE('',#5112,#5295,#2780,.T.);
#6702=EDGE_CURVE('',#5113,#5294,#2781,.T.);
#6703=EDGE_CURVE('',#5114,#5293,#2782,.T.);
#6704=EDGE_CURVE('',#5115,#5292,#2783,.T.);
#6705=EDGE_CURVE('',#5116,#5291,#2784,.T.);
#6706=EDGE_CURVE('',#5117,#5290,#2785,.T.);
#6707=EDGE_CURVE('',#5118,#5289,#2786,.T.);
#6708=EDGE_CURVE('',#5119,#5288,#2787,.T.);
#6709=EDGE_CURVE('',#5120,#5287,#2788,.T.);
#6710=EDGE_CURVE('',#5121,#5286,#2789,.T.);
#6711=EDGE_CURVE('',#5122,#5285,#2790,.T.);
#6712=EDGE_CURVE('',#5123,#5284,#2791,.T.);
#6713=EDGE_CURVE('',#5124,#5283,#2792,.T.);
#6714=EDGE_CURVE('',#5125,#5282,#2793,.T.);
#6715=EDGE_CURVE('',#5126,#5281,#2794,.T.);
#6716=EDGE_CURVE('',#5127,#5280,#2795,.T.);
#6717=EDGE_CURVE('',#5128,#5279,#2796,.T.);
#6718=EDGE_CURVE('',#5129,#5278,#2797,.T.);
#6719=EDGE_CURVE('',#5130,#5277,#2798,.T.);
#6720=EDGE_CURVE('',#5131,#5276,#2799,.T.);
#6721=EDGE_CURVE('',#5132,#5275,#2800,.T.);
#6722=EDGE_CURVE('',#5133,#5274,#2801,.T.);
#6723=EDGE_CURVE('',#5134,#5273,#2802,.T.);
#6724=EDGE_CURVE('',#5135,#5272,#2803,.T.);
#6725=EDGE_CURVE('',#5136,#5271,#2804,.T.);
#6726=EDGE_CURVE('',#5137,#5270,#2805,.T.);
#6727=EDGE_CURVE('',#5138,#5269,#2806,.T.);
#6728=EDGE_CURVE('',#5139,#5268,#2807,.T.);
#6729=EDGE_CURVE('',#5140,#5267,#2808,.T.);
#6730=EDGE_CURVE('',#5141,#5266,#2809,.T.);
#6731=EDGE_CURVE('',#5142,#5265,#2810,.T.);
#6732=EDGE_CURVE('',#5143,#5264,#2811,.T.);
#6733=EDGE_CURVE('',#5144,#5263,#2812,.T.);
#6734=EDGE_CURVE('',#5145,#5262,#2813,.T.);
#6735=EDGE_CURVE('',#5146,#5261,#2814,.T.);
#6736=EDGE_CURVE('',#5147,#5260,#2815,.T.);
#6737=EDGE_CURVE('',#5148,#5259,#2816,.T.);
#6738=EDGE_CURVE('',#5149,#5258,#2817,.T.);
#6739=EDGE_CURVE('',#5150,#5257,#2818,.T.);
#6740=EDGE_CURVE('',#5151,#5256,#2819,.T.);
#6741=EDGE_CURVE('',#5152,#5255,#2820,.T.);
#6742=EDGE_CURVE('',#5153,#5254,#2821,.T.);
#6743=EDGE_CURVE('',#5154,#5253,#2822,.T.);
#6744=EDGE_CURVE('',#5155,#5252,#2823,.T.);
#6745=EDGE_CURVE('',#5156,#5251,#2824,.T.);
#6746=EDGE_CURVE('',#5157,#5250,#2825,.T.);
#6747=EDGE_CURVE('',#5158,#5249,#2826,.T.);
#6748=EDGE_CURVE('',#5159,#5248,#2827,.T.);
#6749=EDGE_CURVE('',#5160,#5247,#2828,.T.);
#6750=EDGE_CURVE('',#5161,#5246,#2829,.T.);
#6751=EDGE_CURVE('',#5162,#5245,#2830,.T.);
#6752=EDGE_CURVE('',#5163,#5244,#2831,.T.);
#6753=EDGE_CURVE('',#5164,#5243,#2832,.T.);
#6754=EDGE_CURVE('',#5165,#5242,#2833,.T.);
#6755=EDGE_CURVE('',#5166,#5241,#2834,.T.);
#6756=EDGE_CURVE('',#5167,#5240,#2835,.T.);
#6757=EDGE_CURVE('',#5168,#5239,#2836,.T.);
#6758=EDGE_CURVE('',#5169,#5238,#2837,.T.);
#6759=EDGE_CURVE('',#5170,#5237,#2838,.T.);
#6760=EDGE_CURVE('',#5171,#5236,#2839,.T.);
#6761=EDGE_CURVE('',#5172,#5235,#2840,.T.);
#6762=EDGE_CURVE('',#5173,#5234,#2841,.T.);
#6763=EDGE_CURVE('',#5174,#5233,#2842,.T.);
#6764=EDGE_CURVE('',#5175,#5232,#2843,.T.);
#6765=EDGE_CURVE('',#5176,#5231,#2844,.T.);
#6766=EDGE_CURVE('',#5177,#5230,#2845,.T.);
#6767=EDGE_CURVE('',#5178,#5229,#2846,.T.);
#6768=EDGE_CURVE('',#5179,#5228,#2847,.T.);
#6769=EDGE_CURVE('',#5182,#5342,#2848,.T.);
#6770=EDGE_CURVE('',#5180,#5343,#2849,.T.);
#6771=EDGE_CURVE('',#5181,#5344,#2850,.T.);
#6772=EDGE_CURVE('',#5187,#5345,#2851,.T.);
#6773=EDGE_CURVE('',#5186,#5346,#2852,.T.);
#6774=EDGE_CURVE('',#5185,#5347,#2853,.T.);
#6775=EDGE_CURVE('',#5184,#5348,#2854,.T.);
#6776=EDGE_CURVE('',#5183,#5349,#2855,.T.);
#6777=EDGE_CURVE('',#5190,#5374,#2856,.T.);
#6778=EDGE_CURVE('',#5188,#5375,#2857,.T.);
#6779=EDGE_CURVE('',#5189,#5376,#2858,.T.);
#6780=EDGE_CURVE('',#5201,#5377,#2859,.T.);
#6781=EDGE_CURVE('',#5200,#5378,#2860,.T.);
#6782=EDGE_CURVE('',#5199,#5379,#2861,.T.);
#6783=EDGE_CURVE('',#5198,#5380,#2862,.T.);
#6784=EDGE_CURVE('',#5197,#5381,#2863,.T.);
#6785=EDGE_CURVE('',#5196,#5382,#2864,.T.);
#6786=EDGE_CURVE('',#5195,#5383,#2865,.T.);
#6787=EDGE_CURVE('',#5194,#5384,#2866,.T.);
#6788=EDGE_CURVE('',#5193,#5385,#2867,.T.);
#6789=EDGE_CURVE('',#5192,#5386,#2868,.T.);
#6790=EDGE_CURVE('',#5191,#5387,#2869,.T.);
#6791=EDGE_CURVE('',#5204,#5350,#2870,.T.);
#6792=EDGE_CURVE('',#5202,#5351,#2871,.T.);
#6793=EDGE_CURVE('',#5203,#5352,#2872,.T.);
#6794=EDGE_CURVE('',#5209,#5353,#2873,.T.);
#6795=EDGE_CURVE('',#5208,#5354,#2874,.T.);
#6796=EDGE_CURVE('',#5207,#5355,#2875,.T.);
#6797=EDGE_CURVE('',#5206,#5356,#2876,.T.);
#6798=EDGE_CURVE('',#5205,#5357,#2877,.T.);
#6799=EDGE_CURVE('',#5212,#5366,#2878,.T.);
#6800=EDGE_CURVE('',#5210,#5367,#2879,.T.);
#6801=EDGE_CURVE('',#5211,#5368,#2880,.T.);
#6802=EDGE_CURVE('',#5217,#5369,#2881,.T.);
#6803=EDGE_CURVE('',#5216,#5370,#2882,.T.);
#6804=EDGE_CURVE('',#5215,#5371,#2883,.T.);
#6805=EDGE_CURVE('',#5214,#5372,#2884,.T.);
#6806=EDGE_CURVE('',#5213,#5373,#2885,.T.);
#6807=EDGE_CURVE('',#5220,#5358,#2886,.T.);
#6808=EDGE_CURVE('',#5218,#5359,#2887,.T.);
#6809=EDGE_CURVE('',#5219,#5360,#2888,.T.);
#6810=EDGE_CURVE('',#5225,#5361,#2889,.T.);
#6811=EDGE_CURVE('',#5224,#5362,#2890,.T.);
#6812=EDGE_CURVE('',#5223,#5363,#2891,.T.);
#6813=EDGE_CURVE('',#5222,#5364,#2892,.T.);
#6814=EDGE_CURVE('',#5221,#5365,#2893,.T.);
#6815=EDGE_CURVE('',#5388,#5388,#4448,.T.);
#6816=EDGE_CURVE('',#5388,#5389,#2894,.T.);
#6817=EDGE_CURVE('',#5389,#5389,#4449,.T.);
#6818=EDGE_CURVE('',#5390,#5390,#4450,.T.);
#6819=EDGE_CURVE('',#5390,#5391,#2895,.T.);
#6820=EDGE_CURVE('',#5391,#5391,#4451,.T.);
#6821=EDGE_CURVE('',#5392,#5393,#2896,.T.);
#6822=EDGE_CURVE('',#5392,#5394,#2897,.T.);
#6823=EDGE_CURVE('',#5395,#5394,#2898,.T.);
#6824=EDGE_CURVE('',#5396,#5395,#2899,.T.);
#6825=EDGE_CURVE('',#5396,#5393,#4452,.T.);
#6826=EDGE_CURVE('',#5397,#5398,#2900,.T.);
#6827=EDGE_CURVE('',#5398,#5399,#2901,.T.);
#6828=EDGE_CURVE('',#5399,#5400,#2902,.T.);
#6829=EDGE_CURVE('',#5401,#5400,#2903,.T.);
#6830=EDGE_CURVE('',#5401,#5397,#4453,.T.);
#6831=EDGE_CURVE('',#5402,#5403,#2904,.T.);
#6832=EDGE_CURVE('',#5402,#5404,#2905,.T.);
#6833=EDGE_CURVE('',#5405,#5404,#2906,.T.);
#6834=EDGE_CURVE('',#5405,#5406,#4454,.T.);
#6835=EDGE_CURVE('',#5403,#5406,#2907,.T.);
#6836=EDGE_CURVE('',#5407,#5400,#2908,.T.);
#6837=EDGE_CURVE('',#5408,#5407,#2909,.T.);
#6838=EDGE_CURVE('',#5408,#5403,#2910,.T.);
#6839=EDGE_CURVE('',#5406,#5409,#2911,.T.);
#6840=EDGE_CURVE('',#5410,#5409,#2912,.T.);
#6841=EDGE_CURVE('',#5410,#5401,#2913,.T.);
#6842=EDGE_CURVE('',#5409,#5411,#4455,.T.);
#6843=EDGE_CURVE('',#5412,#5411,#2914,.T.);
#6844=EDGE_CURVE('',#5412,#5413,#2915,.T.);
#6845=EDGE_CURVE('',#5413,#5414,#2916,.T.);
#6846=EDGE_CURVE('',#5414,#5410,#4456,.T.);
#6847=EDGE_CURVE('',#5415,#5416,#2917,.T.);
#6848=EDGE_CURVE('',#5415,#5417,#2918,.T.);
#6849=EDGE_CURVE('',#5417,#5418,#2919,.T.);
#6850=EDGE_CURVE('',#5418,#5419,#2920,.T.);
#6851=EDGE_CURVE('',#5419,#5420,#2921,.T.);
#6852=EDGE_CURVE('',#5420,#5421,#2922,.T.);
#6853=EDGE_CURVE('',#5421,#5422,#2923,.T.);
#6854=EDGE_CURVE('',#5422,#5416,#2924,.T.);
#6855=EDGE_CURVE('',#5423,#5424,#2925,.T.);
#6856=EDGE_CURVE('',#5424,#5425,#2926,.T.);
#6857=EDGE_CURVE('',#5425,#5426,#2927,.T.);
#6858=EDGE_CURVE('',#5426,#5427,#4457,.T.);
#6859=EDGE_CURVE('',#5423,#5427,#2928,.T.);
#6860=EDGE_CURVE('',#5428,#5429,#2929,.T.);
#6861=EDGE_CURVE('',#5428,#5396,#2930,.T.);
#6862=EDGE_CURVE('',#5430,#5395,#2931,.T.);
#6863=EDGE_CURVE('',#5431,#5430,#2932,.T.);
#6864=EDGE_CURVE('',#5431,#5423,#2933,.T.);
#6865=EDGE_CURVE('',#5427,#5429,#2934,.T.);
#6866=EDGE_CURVE('',#5432,#5433,#2935,.T.);
#6867=EDGE_CURVE('',#5433,#5428,#4458,.T.);
#6868=EDGE_CURVE('',#5429,#5434,#4459,.T.);
#6869=EDGE_CURVE('',#5435,#5434,#2936,.T.);
#6870=EDGE_CURVE('',#5435,#5432,#2937,.T.);
#6871=EDGE_CURVE('',#5436,#5437,#2938,.T.);
#6872=EDGE_CURVE('',#5437,#5438,#2939,.T.);
#6873=EDGE_CURVE('',#5438,#5439,#2940,.T.);
#6874=EDGE_CURVE('',#5439,#5440,#2941,.T.);
#6875=EDGE_CURVE('',#5440,#5441,#2942,.T.);
#6876=EDGE_CURVE('',#5441,#5442,#2943,.T.);
#6877=EDGE_CURVE('',#5443,#5442,#2944,.T.);
#6878=EDGE_CURVE('',#5443,#5436,#2945,.T.);
#6879=EDGE_CURVE('',#5442,#5398,#4460,.T.);
#6880=EDGE_CURVE('',#5397,#5414,#2946,.T.);
#6881=EDGE_CURVE('',#5413,#5422,#4461,.T.);
#6882=EDGE_CURVE('',#5421,#5392,#4462,.T.);
#6883=EDGE_CURVE('',#5393,#5433,#2947,.T.);
#6884=EDGE_CURVE('',#5432,#5443,#4463,.T.);
#6885=EDGE_CURVE('',#5444,#5445,#4464,.T.);
#6886=EDGE_CURVE('',#5446,#5444,#2948,.T.);
#6887=EDGE_CURVE('',#5447,#5446,#4465,.T.);
#6888=EDGE_CURVE('',#5445,#5447,#2949,.T.);
#6889=EDGE_CURVE('',#5404,#5437,#4466,.T.);
#6890=EDGE_CURVE('',#5436,#5435,#4467,.T.);
#6891=EDGE_CURVE('',#5434,#5426,#2950,.T.);
#6892=EDGE_CURVE('',#5425,#5415,#4468,.T.);
#6893=EDGE_CURVE('',#5416,#5412,#4469,.T.);
#6894=EDGE_CURVE('',#5411,#5405,#2951,.T.);
#6895=EDGE_CURVE('',#5448,#5449,#2952,.T.);
#6896=EDGE_CURVE('',#5449,#5450,#4470,.T.);
#6897=EDGE_CURVE('',#5450,#5451,#2953,.T.);
#6898=EDGE_CURVE('',#5451,#5448,#4471,.T.);
#6899=EDGE_CURVE('',#5450,#5445,#2954,.T.);
#6900=EDGE_CURVE('',#5449,#5444,#2955,.T.);
#6901=EDGE_CURVE('',#5448,#5446,#2956,.T.);
#6902=EDGE_CURVE('',#5451,#5447,#2957,.T.);
#6903=EDGE_CURVE('',#5399,#5441,#4472,.T.);
#6904=EDGE_CURVE('',#5440,#5452,#4473,.T.);
#6905=EDGE_CURVE('',#5452,#5407,#2958,.T.);
#6906=EDGE_CURVE('',#5453,#5408,#2959,.T.);
#6907=EDGE_CURVE('',#5453,#5439,#4474,.T.);
#6908=EDGE_CURVE('',#5438,#5402,#4475,.T.);
#6909=EDGE_CURVE('',#5452,#5453,#2960,.T.);
#6910=EDGE_CURVE('',#5394,#5420,#4476,.T.);
#6911=EDGE_CURVE('',#5419,#5454,#4477,.T.);
#6912=EDGE_CURVE('',#5430,#5454,#2961,.T.);
#6913=EDGE_CURVE('',#5431,#5455,#2962,.T.);
#6914=EDGE_CURVE('',#5455,#5418,#4478,.T.);
#6915=EDGE_CURVE('',#5417,#5424,#4479,.T.);
#6916=EDGE_CURVE('',#5454,#5455,#2963,.T.);
#6917=EDGE_CURVE('',#5456,#5456,#4480,.T.);
#6918=EDGE_CURVE('',#5456,#5457,#2964,.T.);
#6919=EDGE_CURVE('',#5457,#5457,#4481,.T.);
#6920=EDGE_CURVE('',#5458,#5458,#4482,.T.);
#6921=EDGE_CURVE('',#5458,#5459,#2965,.T.);
#6922=EDGE_CURVE('',#5459,#5459,#4483,.T.);
#6923=EDGE_CURVE('',#5460,#5461,#2966,.T.);
#6924=EDGE_CURVE('',#5460,#5462,#4484,.T.);
#6925=EDGE_CURVE('',#5463,#5462,#2967,.T.);
#6926=EDGE_CURVE('',#5463,#5464,#4485,.T.);
#6927=EDGE_CURVE('',#5465,#5464,#2968,.T.);
#6928=EDGE_CURVE('',#5461,#5465,#2969,.T.);
#6929=EDGE_CURVE('',#5466,#5467,#2970,.T.);
#6930=EDGE_CURVE('',#5468,#5466,#2971,.T.);
#6931=EDGE_CURVE('',#5469,#5468,#2972,.T.);
#6932=EDGE_CURVE('',#5470,#5469,#2973,.T.);
#6933=EDGE_CURVE('',#5471,#5470,#2974,.T.);
#6934=EDGE_CURVE('',#5471,#5472,#2975,.T.);
#6935=EDGE_CURVE('',#5473,#5472,#2976,.T.);
#6936=EDGE_CURVE('',#5467,#5473,#2977,.T.);
#6937=EDGE_CURVE('',#5474,#5472,#2978,.T.);
#6938=EDGE_CURVE('',#5475,#5474,#2979,.T.);
#6939=EDGE_CURVE('',#5475,#5473,#2980,.T.);
#6940=EDGE_CURVE('',#5469,#5476,#2981,.T.);
#6941=EDGE_CURVE('',#5477,#5468,#2982,.T.);
#6942=EDGE_CURVE('',#5476,#5477,#2983,.T.);
#6943=EDGE_CURVE('',#5478,#5475,#2984,.T.);
#6944=EDGE_CURVE('',#5478,#5460,#2985,.T.);
#6945=EDGE_CURVE('',#5479,#5461,#2986,.T.);
#6946=EDGE_CURVE('',#5480,#5479,#2987,.T.);
#6947=EDGE_CURVE('',#5480,#5467,#2988,.T.);
#6948=EDGE_CURVE('',#5464,#5481,#2989,.T.);
#6949=EDGE_CURVE('',#5477,#5481,#2990,.T.);
#6950=EDGE_CURVE('',#5482,#5466,#2991,.T.);
#6951=EDGE_CURVE('',#5483,#5482,#2992,.T.);
#6952=EDGE_CURVE('',#5483,#5465,#2993,.T.);
#6953=EDGE_CURVE('',#5462,#5484,#2994,.T.);
#6954=EDGE_CURVE('',#5485,#5484,#2995,.T.);
#6955=EDGE_CURVE('',#5485,#5463,#2996,.T.);
#6956=EDGE_CURVE('',#5484,#5478,#4486,.T.);
#6957=EDGE_CURVE('',#5486,#5474,#2997,.T.);
#6958=EDGE_CURVE('',#5487,#5486,#2998,.T.);
#6959=EDGE_CURVE('',#5487,#5476,#2999,.T.);
#6960=EDGE_CURVE('',#5481,#5485,#4487,.T.);
#6961=EDGE_CURVE('',#5486,#5471,#3000,.T.);
#6962=EDGE_CURVE('',#5470,#5487,#3001,.T.);
#6963=EDGE_CURVE('',#5482,#5480,#3002,.T.);
#6964=EDGE_CURVE('',#5479,#5483,#3003,.T.);
#6965=EDGE_CURVE('',#5488,#5489,#3004,.T.);
#6966=EDGE_CURVE('',#5489,#5490,#4488,.T.);
#6967=EDGE_CURVE('',#5490,#5491,#3005,.T.);
#6968=EDGE_CURVE('',#5491,#5492,#4489,.T.);
#6969=EDGE_CURVE('',#5492,#5493,#3006,.T.);
#6970=EDGE_CURVE('',#5493,#5494,#4490,.T.);
#6971=EDGE_CURVE('',#5494,#5495,#3007,.T.);
#6972=EDGE_CURVE('',#5495,#5488,#4491,.T.);
#6973=EDGE_CURVE('',#5496,#5497,#3008,.T.);
#6974=EDGE_CURVE('',#5498,#5496,#3009,.T.);
#6975=EDGE_CURVE('',#5499,#5498,#3010,.T.);
#6976=EDGE_CURVE('',#5497,#5499,#3011,.T.);
#6977=EDGE_CURVE('',#5500,#5501,#3012,.T.);
#6978=EDGE_CURVE('',#5500,#5502,#4492,.T.);
#6979=EDGE_CURVE('',#5503,#5502,#3013,.T.);
#6980=EDGE_CURVE('',#5503,#5504,#4493,.T.);
#6981=EDGE_CURVE('',#5505,#5504,#3014,.T.);
#6982=EDGE_CURVE('',#5505,#5506,#4494,.T.);
#6983=EDGE_CURVE('',#5507,#5506,#3015,.T.);
#6984=EDGE_CURVE('',#5507,#5501,#4495,.T.);
#6985=EDGE_CURVE('',#5508,#5509,#3016,.T.);
#6986=EDGE_CURVE('',#5509,#5510,#3017,.T.);
#6987=EDGE_CURVE('',#5510,#5511,#3018,.T.);
#6988=EDGE_CURVE('',#5511,#5508,#3019,.T.);
#6989=EDGE_CURVE('',#5490,#5500,#3020,.T.);
#6990=EDGE_CURVE('',#5501,#5491,#3021,.T.);
#6991=EDGE_CURVE('',#5492,#5507,#3022,.T.);
#6992=EDGE_CURVE('',#5506,#5493,#3023,.T.);
#6993=EDGE_CURVE('',#5504,#5495,#3024,.T.);
#6994=EDGE_CURVE('',#5494,#5505,#3025,.T.);
#6995=EDGE_CURVE('',#5502,#5489,#3026,.T.);
#6996=EDGE_CURVE('',#5488,#5503,#3027,.T.);
#6997=EDGE_CURVE('',#5498,#5508,#3028,.T.);
#6998=EDGE_CURVE('',#5496,#5509,#3029,.T.);
#6999=EDGE_CURVE('',#5497,#5510,#3030,.T.);
#7000=EDGE_CURVE('',#5499,#5511,#3031,.T.);
#7001=EDGE_CURVE('',#5512,#5512,#4496,.T.);
#7002=EDGE_CURVE('',#5512,#5513,#3032,.T.);
#7003=EDGE_CURVE('',#5513,#5513,#4497,.T.);
#7004=EDGE_CURVE('',#5514,#5515,#4498,.T.);
#7005=EDGE_CURVE('',#5515,#5514,#4499,.T.);
#7006=EDGE_CURVE('',#5515,#5516,#3033,.T.);
#7007=EDGE_CURVE('',#5516,#5516,#4500,.T.);
#7008=EDGE_CURVE('',#5514,#5517,#3034,.T.);
#7009=EDGE_CURVE('',#5517,#5517,#4501,.T.);
#7010=EDGE_CURVE('',#5518,#5518,#4502,.T.);
#7011=EDGE_CURVE('',#5518,#5519,#3035,.T.);
#7012=EDGE_CURVE('',#5519,#5519,#4503,.T.);
#7013=EDGE_CURVE('',#5520,#5520,#4504,.T.);
#7014=EDGE_CURVE('',#5520,#5521,#3036,.T.);
#7015=EDGE_CURVE('',#5521,#5521,#4505,.T.);
#7016=EDGE_CURVE('',#5522,#5522,#4506,.T.);
#7017=EDGE_CURVE('',#5522,#5523,#3037,.T.);
#7018=EDGE_CURVE('',#5523,#5523,#4507,.T.);
#7019=EDGE_CURVE('',#5524,#5524,#4508,.T.);
#7020=EDGE_CURVE('',#5524,#5525,#3038,.T.);
#7021=EDGE_CURVE('',#5525,#5525,#4509,.T.);
#7022=EDGE_CURVE('',#5526,#5527,#4510,.T.);
#7023=EDGE_CURVE('',#5528,#5529,#4511,.T.);
#7024=EDGE_CURVE('',#5530,#5531,#4512,.T.);
#7025=EDGE_CURVE('',#5532,#5533,#4513,.T.);
#7026=EDGE_CURVE('',#5534,#5535,#4514,.T.);
#7027=EDGE_CURVE('',#5536,#5537,#4515,.T.);
#7028=EDGE_CURVE('',#5538,#5539,#4516,.T.);
#7029=EDGE_CURVE('',#5540,#5540,#4517,.T.);
#7030=EDGE_CURVE('',#5540,#5541,#4518,.T.);
#7031=EDGE_CURVE('',#5541,#5541,#4519,.T.);
#7032=EDGE_CURVE('',#5542,#5542,#4520,.T.);
#7033=EDGE_CURVE('',#5542,#5540,#3039,.T.);
#7034=EDGE_CURVE('',#5543,#5543,#4521,.T.);
#7035=EDGE_CURVE('',#5543,#5542,#4522,.T.);
#7036=EDGE_CURVE('',#5544,#5544,#4523,.T.);
#7037=EDGE_CURVE('',#5544,#5545,#3040,.T.);
#7038=EDGE_CURVE('',#5545,#5545,#4524,.T.);
#7039=EDGE_CURVE('',#5546,#5546,#4525,.T.);
#7040=EDGE_CURVE('',#5546,#5544,#4526,.T.);
#7041=EDGE_CURVE('',#5547,#5547,#4527,.T.);
#7042=EDGE_CURVE('',#5547,#5546,#3041,.T.);
#7043=EDGE_CURVE('',#5548,#5548,#4528,.T.);
#7044=EDGE_CURVE('',#5548,#5547,#3042,.T.);
#7045=EDGE_CURVE('',#5549,#5549,#4529,.T.);
#7046=EDGE_CURVE('',#5549,#5548,#4530,.T.);
#7047=EDGE_CURVE('',#5550,#5551,#4531,.T.);
#7048=EDGE_CURVE('',#5551,#5550,#4532,.T.);
#7049=EDGE_CURVE('',#5551,#5549,#3043,.T.);
#7050=EDGE_CURVE('',#5550,#5552,#3044,.T.);
#7051=EDGE_CURVE('',#5553,#5552,#4533,.T.);
#7052=EDGE_CURVE('',#5552,#5553,#4534,.T.);
#7053=EDGE_CURVE('',#5554,#5554,#4535,.T.);
#7054=EDGE_CURVE('',#5554,#5553,#4536,.T.);
#7055=EDGE_CURVE('',#5555,#5555,#4537,.T.);
#7056=EDGE_CURVE('',#5555,#5554,#3045,.T.);
#7057=EDGE_CURVE('',#5556,#5556,#4538,.T.);
#7058=EDGE_CURVE('',#5556,#5557,#4539,.T.);
#7059=EDGE_CURVE('',#5557,#5557,#4540,.T.);
#7060=EDGE_CURVE('',#5558,#5558,#4541,.T.);
#7061=EDGE_CURVE('',#5558,#5559,#3046,.T.);
#7062=EDGE_CURVE('',#5559,#5559,#4542,.T.);
#7063=EDGE_CURVE('',#5560,#5560,#4543,.T.);
#7064=EDGE_CURVE('',#5560,#5558,#3047,.T.);
#7065=EDGE_CURVE('',#5561,#5562,#4544,.T.);
#7066=EDGE_CURVE('',#5562,#5561,#4545,.T.);
#7067=EDGE_CURVE('',#5562,#5560,#3048,.T.);
#7068=EDGE_CURVE('',#5561,#5563,#3049,.T.);
#7069=EDGE_CURVE('',#5563,#5563,#4546,.T.);
#7070=EDGE_CURVE('',#5564,#5565,#4547,.T.);
#7071=EDGE_CURVE('',#5565,#5566,#3050,.T.);
#7072=EDGE_CURVE('',#5566,#5566,#4548,.T.);
#7073=EDGE_CURVE('',#5565,#5564,#4549,.T.);
#7074=EDGE_CURVE('',#5567,#5568,#4550,.T.);
#7075=EDGE_CURVE('',#5568,#5569,#3051,.T.);
#7076=EDGE_CURVE('',#5569,#5569,#4551,.T.);
#7077=EDGE_CURVE('',#5568,#5567,#4552,.T.);
#7078=EDGE_CURVE('',#5570,#5570,#4553,.T.);
#7079=EDGE_CURVE('',#5570,#5571,#3052,.T.);
#7080=EDGE_CURVE('',#5571,#5571,#4554,.T.);
#7081=EDGE_CURVE('',#5572,#5573,#4555,.T.);
#7082=EDGE_CURVE('',#5573,#5572,#4556,.T.);
#7083=EDGE_CURVE('',#5573,#5574,#3053,.T.);
#7084=EDGE_CURVE('',#5574,#5574,#4557,.T.);
#7085=EDGE_CURVE('',#5572,#5575,#3054,.T.);
#7086=EDGE_CURVE('',#5576,#5575,#4558,.T.);
#7087=EDGE_CURVE('',#5575,#5576,#4559,.T.);
#7088=EDGE_CURVE('',#5567,#5576,#3055,.T.);
#7089=EDGE_CURVE('',#5557,#5570,#3056,.T.);
#7090=EDGE_CURVE('',#5577,#5577,#4560,.T.);
#7091=EDGE_CURVE('',#5577,#5578,#3057,.T.);
#7092=EDGE_CURVE('',#5578,#5578,#4561,.T.);
#7093=EDGE_CURVE('',#5579,#5579,#4562,.T.);
#7094=EDGE_CURVE('',#5579,#5577,#4563,.T.);
#7095=EDGE_CURVE('',#5580,#5580,#4564,.T.);
#7096=EDGE_CURVE('',#5580,#5581,#4565,.T.);
#7097=EDGE_CURVE('',#5581,#5581,#4566,.T.);
#7098=EDGE_CURVE('',#5582,#5582,#4567,.T.);
#7099=EDGE_CURVE('',#5582,#5580,#3058,.T.);
#7100=EDGE_CURVE('',#5583,#5583,#4568,.T.);
#7101=EDGE_CURVE('',#5583,#5582,#4569,.T.);
#7102=EDGE_CURVE('',#5584,#5584,#4570,.T.);
#7103=EDGE_CURVE('',#5584,#5585,#4571,.T.);
#7104=EDGE_CURVE('',#5585,#5585,#4572,.T.);
#7105=EDGE_CURVE('',#5586,#5586,#4573,.T.);
#7106=EDGE_CURVE('',#5586,#5584,#3059,.T.);
#7107=EDGE_CURVE('',#5564,#5556,#3060,.T.);
#7108=ORIENTED_EDGE('',*,*,#5587,.F.);
#7109=ORIENTED_EDGE('',*,*,#5588,.T.);
#7110=ORIENTED_EDGE('',*,*,#5589,.T.);
#7111=ORIENTED_EDGE('',*,*,#5588,.F.);
#7112=ORIENTED_EDGE('',*,*,#5590,.F.);
#7113=ORIENTED_EDGE('',*,*,#5591,.T.);
#7114=ORIENTED_EDGE('',*,*,#5592,.T.);
#7115=ORIENTED_EDGE('',*,*,#5591,.F.);
#7116=ORIENTED_EDGE('',*,*,#5593,.F.);
#7117=ORIENTED_EDGE('',*,*,#5594,.T.);
#7118=ORIENTED_EDGE('',*,*,#5595,.T.);
#7119=ORIENTED_EDGE('',*,*,#5594,.F.);
#7120=ORIENTED_EDGE('',*,*,#5596,.T.);
#7121=ORIENTED_EDGE('',*,*,#5597,.T.);
#7122=ORIENTED_EDGE('',*,*,#5598,.T.);
#7123=ORIENTED_EDGE('',*,*,#5597,.F.);
#7124=ORIENTED_EDGE('',*,*,#5599,.F.);
#7125=ORIENTED_EDGE('',*,*,#5600,.T.);
#7126=ORIENTED_EDGE('',*,*,#5601,.T.);
#7127=ORIENTED_EDGE('',*,*,#5600,.F.);
#7128=ORIENTED_EDGE('',*,*,#5602,.T.);
#7129=ORIENTED_EDGE('',*,*,#5603,.T.);
#7130=ORIENTED_EDGE('',*,*,#5604,.T.);
#7131=ORIENTED_EDGE('',*,*,#5603,.F.);
#7132=ORIENTED_EDGE('',*,*,#5605,.F.);
#7133=ORIENTED_EDGE('',*,*,#5606,.T.);
#7134=ORIENTED_EDGE('',*,*,#5607,.T.);
#7135=ORIENTED_EDGE('',*,*,#5606,.F.);
#7136=ORIENTED_EDGE('',*,*,#5608,.F.);
#7137=ORIENTED_EDGE('',*,*,#5609,.T.);
#7138=ORIENTED_EDGE('',*,*,#5610,.T.);
#7139=ORIENTED_EDGE('',*,*,#5609,.F.);
#7140=ORIENTED_EDGE('',*,*,#5611,.F.);
#7141=ORIENTED_EDGE('',*,*,#5612,.T.);
#7142=ORIENTED_EDGE('',*,*,#5613,.T.);
#7143=ORIENTED_EDGE('',*,*,#5612,.F.);
#7144=ORIENTED_EDGE('',*,*,#5614,.F.);
#7145=ORIENTED_EDGE('',*,*,#5615,.F.);
#7146=ORIENTED_EDGE('',*,*,#5616,.T.);
#7147=ORIENTED_EDGE('',*,*,#5617,.T.);
#7148=ORIENTED_EDGE('',*,*,#5618,.T.);
#7149=ORIENTED_EDGE('',*,*,#5619,.F.);
#7150=ORIENTED_EDGE('',*,*,#5620,.T.);
#7151=ORIENTED_EDGE('',*,*,#5621,.F.);
#7152=ORIENTED_EDGE('',*,*,#5622,.T.);
#7153=ORIENTED_EDGE('',*,*,#5623,.T.);
#7154=ORIENTED_EDGE('',*,*,#5624,.F.);
#7155=ORIENTED_EDGE('',*,*,#5623,.F.);
#7156=ORIENTED_EDGE('',*,*,#5625,.T.);
#7157=ORIENTED_EDGE('',*,*,#5626,.T.);
#7158=ORIENTED_EDGE('',*,*,#5627,.T.);
#7159=ORIENTED_EDGE('',*,*,#5628,.F.);
#7160=ORIENTED_EDGE('',*,*,#5629,.T.);
#7161=ORIENTED_EDGE('',*,*,#5630,.T.);
#7162=ORIENTED_EDGE('',*,*,#5631,.F.);
#7163=ORIENTED_EDGE('',*,*,#5617,.F.);
#7164=ORIENTED_EDGE('',*,*,#5632,.T.);
#7165=ORIENTED_EDGE('',*,*,#5633,.T.);
#7166=ORIENTED_EDGE('',*,*,#5634,.T.);
#7167=ORIENTED_EDGE('',*,*,#5635,.T.);
#7168=ORIENTED_EDGE('',*,*,#5636,.F.);
#7169=ORIENTED_EDGE('',*,*,#5637,.T.);
#7170=ORIENTED_EDGE('',*,*,#5621,.T.);
#7171=ORIENTED_EDGE('',*,*,#5638,.F.);
#7172=ORIENTED_EDGE('',*,*,#5639,.F.);
#7173=ORIENTED_EDGE('',*,*,#5640,.F.);
#7174=ORIENTED_EDGE('',*,*,#5641,.F.);
#7175=ORIENTED_EDGE('',*,*,#5642,.F.);
#7176=ORIENTED_EDGE('',*,*,#5643,.F.);
#7177=ORIENTED_EDGE('',*,*,#5644,.F.);
#7178=ORIENTED_EDGE('',*,*,#5645,.F.);
#7179=ORIENTED_EDGE('',*,*,#5646,.F.);
#7180=ORIENTED_EDGE('',*,*,#5647,.F.);
#7181=ORIENTED_EDGE('',*,*,#5648,.F.);
#7182=ORIENTED_EDGE('',*,*,#5649,.F.);
#7183=ORIENTED_EDGE('',*,*,#5650,.F.);
#7184=ORIENTED_EDGE('',*,*,#5651,.F.);
#7185=ORIENTED_EDGE('',*,*,#5613,.F.);
#7186=ORIENTED_EDGE('',*,*,#5637,.F.);
#7187=ORIENTED_EDGE('',*,*,#5652,.F.);
#7188=ORIENTED_EDGE('',*,*,#5653,.T.);
#7189=ORIENTED_EDGE('',*,*,#5654,.T.);
#7190=ORIENTED_EDGE('',*,*,#5622,.F.);
#7191=ORIENTED_EDGE('',*,*,#5636,.T.);
#7192=ORIENTED_EDGE('',*,*,#5655,.F.);
#7193=ORIENTED_EDGE('',*,*,#5656,.F.);
#7194=ORIENTED_EDGE('',*,*,#5652,.T.);
#7195=ORIENTED_EDGE('',*,*,#5631,.T.);
#7196=ORIENTED_EDGE('',*,*,#5657,.T.);
#7197=ORIENTED_EDGE('',*,*,#5658,.T.);
#7198=ORIENTED_EDGE('',*,*,#5655,.T.);
#7199=ORIENTED_EDGE('',*,*,#5635,.F.);
#7200=ORIENTED_EDGE('',*,*,#5659,.T.);
#7201=ORIENTED_EDGE('',*,*,#5660,.T.);
#7202=ORIENTED_EDGE('',*,*,#5618,.F.);
#7203=ORIENTED_EDGE('',*,*,#5661,.T.);
#7204=ORIENTED_EDGE('',*,*,#5629,.F.);
#7205=ORIENTED_EDGE('',*,*,#5662,.F.);
#7206=ORIENTED_EDGE('',*,*,#5663,.F.);
#7207=ORIENTED_EDGE('',*,*,#5664,.T.);
#7208=ORIENTED_EDGE('',*,*,#5627,.F.);
#7209=ORIENTED_EDGE('',*,*,#5665,.T.);
#7210=ORIENTED_EDGE('',*,*,#5666,.F.);
#7211=ORIENTED_EDGE('',*,*,#5667,.T.);
#7212=ORIENTED_EDGE('',*,*,#5625,.F.);
#7213=ORIENTED_EDGE('',*,*,#5654,.F.);
#7214=ORIENTED_EDGE('',*,*,#5668,.F.);
#7215=ORIENTED_EDGE('',*,*,#5666,.T.);
#7216=ORIENTED_EDGE('',*,*,#5669,.T.);
#7217=ORIENTED_EDGE('',*,*,#5668,.T.);
#7218=ORIENTED_EDGE('',*,*,#5653,.F.);
#7219=ORIENTED_EDGE('',*,*,#5656,.T.);
#7220=ORIENTED_EDGE('',*,*,#5658,.F.);
#7221=ORIENTED_EDGE('',*,*,#5670,.T.);
#7222=ORIENTED_EDGE('',*,*,#5587,.T.);
#7223=ORIENTED_EDGE('',*,*,#5590,.T.);
#7224=ORIENTED_EDGE('',*,*,#5595,.F.);
#7225=ORIENTED_EDGE('',*,*,#5601,.F.);
#7226=ORIENTED_EDGE('',*,*,#5605,.T.);
#7227=ORIENTED_EDGE('',*,*,#5611,.T.);
#7228=ORIENTED_EDGE('',*,*,#5610,.F.);
#7229=ORIENTED_EDGE('',*,*,#5608,.T.);
#7230=ORIENTED_EDGE('',*,*,#5607,.F.);
#7231=ORIENTED_EDGE('',*,*,#5638,.T.);
#7232=ORIENTED_EDGE('',*,*,#5620,.F.);
#7233=ORIENTED_EDGE('',*,*,#5671,.F.);
#7234=ORIENTED_EDGE('',*,*,#5672,.T.);
#7235=ORIENTED_EDGE('',*,*,#5673,.F.);
#7236=ORIENTED_EDGE('',*,*,#5674,.T.);
#7237=ORIENTED_EDGE('',*,*,#5639,.T.);
#7238=ORIENTED_EDGE('',*,*,#5672,.F.);
#7239=ORIENTED_EDGE('',*,*,#5675,.F.);
#7240=ORIENTED_EDGE('',*,*,#5676,.T.);
#7241=ORIENTED_EDGE('',*,*,#5677,.T.);
#7242=ORIENTED_EDGE('',*,*,#5673,.T.);
#7243=ORIENTED_EDGE('',*,*,#5671,.T.);
#7244=ORIENTED_EDGE('',*,*,#5619,.T.);
#7245=ORIENTED_EDGE('',*,*,#5660,.F.);
#7246=ORIENTED_EDGE('',*,*,#5626,.F.);
#7247=ORIENTED_EDGE('',*,*,#5667,.F.);
#7248=ORIENTED_EDGE('',*,*,#5669,.F.);
#7249=ORIENTED_EDGE('',*,*,#5665,.F.);
#7250=ORIENTED_EDGE('',*,*,#5630,.F.);
#7251=ORIENTED_EDGE('',*,*,#5661,.F.);
#7252=ORIENTED_EDGE('',*,*,#5670,.F.);
#7253=ORIENTED_EDGE('',*,*,#5657,.F.);
#7254=ORIENTED_EDGE('',*,*,#5599,.T.);
#7255=ORIENTED_EDGE('',*,*,#5604,.F.);
#7256=ORIENTED_EDGE('',*,*,#5593,.T.);
#7257=ORIENTED_EDGE('',*,*,#5598,.F.);
#7258=ORIENTED_EDGE('',*,*,#5647,.T.);
#7259=ORIENTED_EDGE('',*,*,#5678,.F.);
#7260=ORIENTED_EDGE('',*,*,#5679,.F.);
#7261=ORIENTED_EDGE('',*,*,#5680,.T.);
#7262=ORIENTED_EDGE('',*,*,#5648,.T.);
#7263=ORIENTED_EDGE('',*,*,#5680,.F.);
#7264=ORIENTED_EDGE('',*,*,#5681,.F.);
#7265=ORIENTED_EDGE('',*,*,#5682,.T.);
#7266=ORIENTED_EDGE('',*,*,#5649,.T.);
#7267=ORIENTED_EDGE('',*,*,#5682,.F.);
#7268=ORIENTED_EDGE('',*,*,#5683,.F.);
#7269=ORIENTED_EDGE('',*,*,#5684,.T.);
#7270=ORIENTED_EDGE('',*,*,#5650,.T.);
#7271=ORIENTED_EDGE('',*,*,#5684,.F.);
#7272=ORIENTED_EDGE('',*,*,#5685,.F.);
#7273=ORIENTED_EDGE('',*,*,#5686,.T.);
#7274=ORIENTED_EDGE('',*,*,#5651,.T.);
#7275=ORIENTED_EDGE('',*,*,#5686,.F.);
#7276=ORIENTED_EDGE('',*,*,#5687,.F.);
#7277=ORIENTED_EDGE('',*,*,#5688,.T.);
#7278=ORIENTED_EDGE('',*,*,#5646,.T.);
#7279=ORIENTED_EDGE('',*,*,#5688,.F.);
#7280=ORIENTED_EDGE('',*,*,#5689,.F.);
#7281=ORIENTED_EDGE('',*,*,#5678,.T.);
#7282=ORIENTED_EDGE('',*,*,#5679,.T.);
#7283=ORIENTED_EDGE('',*,*,#5689,.T.);
#7284=ORIENTED_EDGE('',*,*,#5687,.T.);
#7285=ORIENTED_EDGE('',*,*,#5685,.T.);
#7286=ORIENTED_EDGE('',*,*,#5683,.T.);
#7287=ORIENTED_EDGE('',*,*,#5681,.T.);
#7288=ORIENTED_EDGE('',*,*,#5592,.F.);
#7289=ORIENTED_EDGE('',*,*,#5641,.T.);
#7290=ORIENTED_EDGE('',*,*,#5690,.F.);
#7291=ORIENTED_EDGE('',*,*,#5691,.F.);
#7292=ORIENTED_EDGE('',*,*,#5692,.T.);
#7293=ORIENTED_EDGE('',*,*,#5642,.T.);
#7294=ORIENTED_EDGE('',*,*,#5692,.F.);
#7295=ORIENTED_EDGE('',*,*,#5693,.F.);
#7296=ORIENTED_EDGE('',*,*,#5694,.T.);
#7297=ORIENTED_EDGE('',*,*,#5643,.T.);
#7298=ORIENTED_EDGE('',*,*,#5694,.F.);
#7299=ORIENTED_EDGE('',*,*,#5695,.F.);
#7300=ORIENTED_EDGE('',*,*,#5696,.T.);
#7301=ORIENTED_EDGE('',*,*,#5644,.T.);
#7302=ORIENTED_EDGE('',*,*,#5696,.F.);
#7303=ORIENTED_EDGE('',*,*,#5697,.F.);
#7304=ORIENTED_EDGE('',*,*,#5698,.T.);
#7305=ORIENTED_EDGE('',*,*,#5645,.T.);
#7306=ORIENTED_EDGE('',*,*,#5698,.F.);
#7307=ORIENTED_EDGE('',*,*,#5699,.F.);
#7308=ORIENTED_EDGE('',*,*,#5700,.T.);
#7309=ORIENTED_EDGE('',*,*,#5640,.T.);
#7310=ORIENTED_EDGE('',*,*,#5700,.F.);
#7311=ORIENTED_EDGE('',*,*,#5701,.F.);
#7312=ORIENTED_EDGE('',*,*,#5690,.T.);
#7313=ORIENTED_EDGE('',*,*,#5691,.T.);
#7314=ORIENTED_EDGE('',*,*,#5701,.T.);
#7315=ORIENTED_EDGE('',*,*,#5699,.T.);
#7316=ORIENTED_EDGE('',*,*,#5697,.T.);
#7317=ORIENTED_EDGE('',*,*,#5695,.T.);
#7318=ORIENTED_EDGE('',*,*,#5693,.T.);
#7319=ORIENTED_EDGE('',*,*,#5589,.F.);
#7320=ORIENTED_EDGE('',*,*,#5677,.F.);
#7321=ORIENTED_EDGE('',*,*,#5702,.T.);
#7322=ORIENTED_EDGE('',*,*,#5632,.F.);
#7323=ORIENTED_EDGE('',*,*,#5674,.F.);
#7324=ORIENTED_EDGE('',*,*,#5634,.F.);
#7325=ORIENTED_EDGE('',*,*,#5703,.T.);
#7326=ORIENTED_EDGE('',*,*,#5675,.T.);
#7327=ORIENTED_EDGE('',*,*,#5659,.F.);
#7328=ORIENTED_EDGE('',*,*,#5633,.F.);
#7329=ORIENTED_EDGE('',*,*,#5702,.F.);
#7330=ORIENTED_EDGE('',*,*,#5676,.F.);
#7331=ORIENTED_EDGE('',*,*,#5703,.F.);
#7332=ORIENTED_EDGE('',*,*,#5615,.T.);
#7333=ORIENTED_EDGE('',*,*,#5704,.T.);
#7334=ORIENTED_EDGE('',*,*,#5663,.T.);
#7335=ORIENTED_EDGE('',*,*,#5705,.T.);
#7336=ORIENTED_EDGE('',*,*,#5602,.F.);
#7337=ORIENTED_EDGE('',*,*,#5596,.F.);
#7338=ORIENTED_EDGE('',*,*,#5624,.T.);
#7339=ORIENTED_EDGE('',*,*,#5664,.F.);
#7340=ORIENTED_EDGE('',*,*,#5704,.F.);
#7341=ORIENTED_EDGE('',*,*,#5614,.T.);
#7342=ORIENTED_EDGE('',*,*,#5628,.T.);
#7343=ORIENTED_EDGE('',*,*,#5616,.F.);
#7344=ORIENTED_EDGE('',*,*,#5705,.F.);
#7345=ORIENTED_EDGE('',*,*,#5662,.T.);
#7346=ORIENTED_EDGE('',*,*,#5706,.T.);
#7347=ORIENTED_EDGE('',*,*,#5707,.T.);
#7348=ORIENTED_EDGE('',*,*,#5708,.F.);
#7349=ORIENTED_EDGE('',*,*,#5707,.F.);
#7350=ORIENTED_EDGE('',*,*,#5709,.T.);
#7351=ORIENTED_EDGE('',*,*,#5710,.T.);
#7352=ORIENTED_EDGE('',*,*,#5711,.F.);
#7353=ORIENTED_EDGE('',*,*,#5710,.F.);
#7354=ORIENTED_EDGE('',*,*,#5712,.T.);
#7355=ORIENTED_EDGE('',*,*,#5713,.T.);
#7356=ORIENTED_EDGE('',*,*,#5714,.F.);
#7357=ORIENTED_EDGE('',*,*,#5713,.F.);
#7358=ORIENTED_EDGE('',*,*,#5715,.F.);
#7359=ORIENTED_EDGE('',*,*,#5716,.T.);
#7360=ORIENTED_EDGE('',*,*,#5717,.F.);
#7361=ORIENTED_EDGE('',*,*,#5716,.F.);
#7362=ORIENTED_EDGE('',*,*,#5718,.T.);
#7363=ORIENTED_EDGE('',*,*,#5719,.T.);
#7364=ORIENTED_EDGE('',*,*,#5720,.F.);
#7365=ORIENTED_EDGE('',*,*,#5719,.F.);
#7366=ORIENTED_EDGE('',*,*,#5721,.F.);
#7367=ORIENTED_EDGE('',*,*,#5722,.T.);
#7368=ORIENTED_EDGE('',*,*,#5723,.F.);
#7369=ORIENTED_EDGE('',*,*,#5722,.F.);
#7370=ORIENTED_EDGE('',*,*,#5724,.T.);
#7371=ORIENTED_EDGE('',*,*,#5725,.T.);
#7372=ORIENTED_EDGE('',*,*,#5726,.F.);
#7373=ORIENTED_EDGE('',*,*,#5725,.F.);
#7374=ORIENTED_EDGE('',*,*,#5727,.T.);
#7375=ORIENTED_EDGE('',*,*,#5728,.T.);
#7376=ORIENTED_EDGE('',*,*,#5729,.F.);
#7377=ORIENTED_EDGE('',*,*,#5728,.F.);
#7378=ORIENTED_EDGE('',*,*,#5730,.T.);
#7379=ORIENTED_EDGE('',*,*,#5731,.T.);
#7380=ORIENTED_EDGE('',*,*,#5732,.F.);
#7381=ORIENTED_EDGE('',*,*,#5731,.F.);
#7382=ORIENTED_EDGE('',*,*,#5733,.T.);
#7383=ORIENTED_EDGE('',*,*,#5734,.F.);
#7384=ORIENTED_EDGE('',*,*,#5735,.F.);
#7385=ORIENTED_EDGE('',*,*,#5736,.T.);
#7386=ORIENTED_EDGE('',*,*,#5737,.F.);
#7387=ORIENTED_EDGE('',*,*,#5738,.T.);
#7388=ORIENTED_EDGE('',*,*,#5739,.F.);
#7389=ORIENTED_EDGE('',*,*,#5740,.F.);
#7390=ORIENTED_EDGE('',*,*,#5741,.F.);
#7391=ORIENTED_EDGE('',*,*,#5742,.T.);
#7392=ORIENTED_EDGE('',*,*,#5743,.T.);
#7393=ORIENTED_EDGE('',*,*,#5744,.F.);
#7394=ORIENTED_EDGE('',*,*,#5745,.F.);
#7395=ORIENTED_EDGE('',*,*,#5746,.F.);
#7396=ORIENTED_EDGE('',*,*,#5734,.T.);
#7397=ORIENTED_EDGE('',*,*,#5747,.T.);
#7398=ORIENTED_EDGE('',*,*,#5740,.T.);
#7399=ORIENTED_EDGE('',*,*,#5748,.T.);
#7400=ORIENTED_EDGE('',*,*,#5749,.F.);
#7401=ORIENTED_EDGE('',*,*,#5750,.F.);
#7402=ORIENTED_EDGE('',*,*,#5751,.F.);
#7403=ORIENTED_EDGE('',*,*,#5752,.T.);
#7404=ORIENTED_EDGE('',*,*,#5753,.T.);
#7405=ORIENTED_EDGE('',*,*,#5736,.F.);
#7406=ORIENTED_EDGE('',*,*,#5754,.F.);
#7407=ORIENTED_EDGE('',*,*,#5755,.T.);
#7408=ORIENTED_EDGE('',*,*,#5756,.F.);
#7409=ORIENTED_EDGE('',*,*,#5757,.F.);
#7410=ORIENTED_EDGE('',*,*,#5758,.F.);
#7411=ORIENTED_EDGE('',*,*,#5759,.T.);
#7412=ORIENTED_EDGE('',*,*,#5760,.T.);
#7413=ORIENTED_EDGE('',*,*,#5761,.T.);
#7414=ORIENTED_EDGE('',*,*,#5762,.T.);
#7415=ORIENTED_EDGE('',*,*,#5763,.T.);
#7416=ORIENTED_EDGE('',*,*,#5764,.T.);
#7417=ORIENTED_EDGE('',*,*,#5765,.T.);
#7418=ORIENTED_EDGE('',*,*,#5766,.T.);
#7419=ORIENTED_EDGE('',*,*,#5767,.T.);
#7420=ORIENTED_EDGE('',*,*,#5768,.T.);
#7421=ORIENTED_EDGE('',*,*,#5769,.T.);
#7422=ORIENTED_EDGE('',*,*,#5770,.T.);
#7423=ORIENTED_EDGE('',*,*,#5732,.T.);
#7424=ORIENTED_EDGE('',*,*,#5754,.T.);
#7425=ORIENTED_EDGE('',*,*,#5735,.T.);
#7426=ORIENTED_EDGE('',*,*,#5771,.F.);
#7427=ORIENTED_EDGE('',*,*,#5772,.F.);
#7428=ORIENTED_EDGE('',*,*,#5773,.T.);
#7429=ORIENTED_EDGE('',*,*,#5755,.F.);
#7430=ORIENTED_EDGE('',*,*,#5773,.F.);
#7431=ORIENTED_EDGE('',*,*,#5774,.T.);
#7432=ORIENTED_EDGE('',*,*,#5775,.T.);
#7433=ORIENTED_EDGE('',*,*,#5748,.F.);
#7434=ORIENTED_EDGE('',*,*,#5739,.T.);
#7435=ORIENTED_EDGE('',*,*,#5776,.F.);
#7436=ORIENTED_EDGE('',*,*,#5777,.F.);
#7437=ORIENTED_EDGE('',*,*,#5756,.T.);
#7438=ORIENTED_EDGE('',*,*,#5775,.F.);
#7439=ORIENTED_EDGE('',*,*,#5778,.F.);
#7440=ORIENTED_EDGE('',*,*,#5779,.F.);
#7441=ORIENTED_EDGE('',*,*,#5780,.F.);
#7442=ORIENTED_EDGE('',*,*,#5781,.T.);
#7443=ORIENTED_EDGE('',*,*,#5782,.F.);
#7444=ORIENTED_EDGE('',*,*,#5744,.T.);
#7445=ORIENTED_EDGE('',*,*,#5783,.F.);
#7446=ORIENTED_EDGE('',*,*,#5784,.T.);
#7447=ORIENTED_EDGE('',*,*,#5785,.T.);
#7448=ORIENTED_EDGE('',*,*,#5750,.T.);
#7449=ORIENTED_EDGE('',*,*,#5786,.F.);
#7450=ORIENTED_EDGE('',*,*,#5787,.T.);
#7451=ORIENTED_EDGE('',*,*,#5771,.T.);
#7452=ORIENTED_EDGE('',*,*,#5746,.T.);
#7453=ORIENTED_EDGE('',*,*,#5781,.F.);
#7454=ORIENTED_EDGE('',*,*,#5788,.F.);
#7455=ORIENTED_EDGE('',*,*,#5778,.T.);
#7456=ORIENTED_EDGE('',*,*,#5774,.F.);
#7457=ORIENTED_EDGE('',*,*,#5772,.T.);
#7458=ORIENTED_EDGE('',*,*,#5787,.F.);
#7459=ORIENTED_EDGE('',*,*,#5789,.F.);
#7460=ORIENTED_EDGE('',*,*,#5706,.F.);
#7461=ORIENTED_EDGE('',*,*,#5709,.F.);
#7462=ORIENTED_EDGE('',*,*,#5714,.T.);
#7463=ORIENTED_EDGE('',*,*,#5720,.T.);
#7464=ORIENTED_EDGE('',*,*,#5724,.F.);
#7465=ORIENTED_EDGE('',*,*,#5730,.F.);
#7466=ORIENTED_EDGE('',*,*,#5729,.T.);
#7467=ORIENTED_EDGE('',*,*,#5727,.F.);
#7468=ORIENTED_EDGE('',*,*,#5726,.T.);
#7469=ORIENTED_EDGE('',*,*,#5753,.F.);
#7470=ORIENTED_EDGE('',*,*,#5790,.F.);
#7471=ORIENTED_EDGE('',*,*,#5791,.T.);
#7472=ORIENTED_EDGE('',*,*,#5737,.T.);
#7473=ORIENTED_EDGE('',*,*,#5792,.T.);
#7474=ORIENTED_EDGE('',*,*,#5790,.T.);
#7475=ORIENTED_EDGE('',*,*,#5752,.F.);
#7476=ORIENTED_EDGE('',*,*,#5793,.F.);
#7477=ORIENTED_EDGE('',*,*,#5794,.T.);
#7478=ORIENTED_EDGE('',*,*,#5776,.T.);
#7479=ORIENTED_EDGE('',*,*,#5738,.F.);
#7480=ORIENTED_EDGE('',*,*,#5791,.F.);
#7481=ORIENTED_EDGE('',*,*,#5792,.F.);
#7482=ORIENTED_EDGE('',*,*,#5795,.F.);
#7483=ORIENTED_EDGE('',*,*,#5796,.F.);
#7484=ORIENTED_EDGE('',*,*,#5745,.T.);
#7485=ORIENTED_EDGE('',*,*,#5782,.T.);
#7486=ORIENTED_EDGE('',*,*,#5789,.T.);
#7487=ORIENTED_EDGE('',*,*,#5786,.T.);
#7488=ORIENTED_EDGE('',*,*,#5749,.T.);
#7489=ORIENTED_EDGE('',*,*,#5779,.T.);
#7490=ORIENTED_EDGE('',*,*,#5788,.T.);
#7491=ORIENTED_EDGE('',*,*,#5780,.T.);
#7492=ORIENTED_EDGE('',*,*,#5718,.F.);
#7493=ORIENTED_EDGE('',*,*,#5723,.T.);
#7494=ORIENTED_EDGE('',*,*,#5712,.F.);
#7495=ORIENTED_EDGE('',*,*,#5717,.T.);
#7496=ORIENTED_EDGE('',*,*,#5770,.F.);
#7497=ORIENTED_EDGE('',*,*,#5797,.F.);
#7498=ORIENTED_EDGE('',*,*,#5798,.T.);
#7499=ORIENTED_EDGE('',*,*,#5799,.T.);
#7500=ORIENTED_EDGE('',*,*,#5769,.F.);
#7501=ORIENTED_EDGE('',*,*,#5800,.F.);
#7502=ORIENTED_EDGE('',*,*,#5801,.T.);
#7503=ORIENTED_EDGE('',*,*,#5797,.T.);
#7504=ORIENTED_EDGE('',*,*,#5768,.F.);
#7505=ORIENTED_EDGE('',*,*,#5802,.F.);
#7506=ORIENTED_EDGE('',*,*,#5803,.T.);
#7507=ORIENTED_EDGE('',*,*,#5800,.T.);
#7508=ORIENTED_EDGE('',*,*,#5767,.F.);
#7509=ORIENTED_EDGE('',*,*,#5804,.F.);
#7510=ORIENTED_EDGE('',*,*,#5805,.T.);
#7511=ORIENTED_EDGE('',*,*,#5802,.T.);
#7512=ORIENTED_EDGE('',*,*,#5766,.F.);
#7513=ORIENTED_EDGE('',*,*,#5806,.F.);
#7514=ORIENTED_EDGE('',*,*,#5807,.T.);
#7515=ORIENTED_EDGE('',*,*,#5804,.T.);
#7516=ORIENTED_EDGE('',*,*,#5765,.F.);
#7517=ORIENTED_EDGE('',*,*,#5799,.F.);
#7518=ORIENTED_EDGE('',*,*,#5808,.T.);
#7519=ORIENTED_EDGE('',*,*,#5806,.T.);
#7520=ORIENTED_EDGE('',*,*,#5798,.F.);
#7521=ORIENTED_EDGE('',*,*,#5801,.F.);
#7522=ORIENTED_EDGE('',*,*,#5803,.F.);
#7523=ORIENTED_EDGE('',*,*,#5805,.F.);
#7524=ORIENTED_EDGE('',*,*,#5807,.F.);
#7525=ORIENTED_EDGE('',*,*,#5808,.F.);
#7526=ORIENTED_EDGE('',*,*,#5711,.T.);
#7527=ORIENTED_EDGE('',*,*,#5764,.F.);
#7528=ORIENTED_EDGE('',*,*,#5809,.F.);
#7529=ORIENTED_EDGE('',*,*,#5810,.T.);
#7530=ORIENTED_EDGE('',*,*,#5811,.T.);
#7531=ORIENTED_EDGE('',*,*,#5763,.F.);
#7532=ORIENTED_EDGE('',*,*,#5812,.F.);
#7533=ORIENTED_EDGE('',*,*,#5813,.T.);
#7534=ORIENTED_EDGE('',*,*,#5809,.T.);
#7535=ORIENTED_EDGE('',*,*,#5762,.F.);
#7536=ORIENTED_EDGE('',*,*,#5814,.F.);
#7537=ORIENTED_EDGE('',*,*,#5815,.T.);
#7538=ORIENTED_EDGE('',*,*,#5812,.T.);
#7539=ORIENTED_EDGE('',*,*,#5761,.F.);
#7540=ORIENTED_EDGE('',*,*,#5816,.F.);
#7541=ORIENTED_EDGE('',*,*,#5817,.T.);
#7542=ORIENTED_EDGE('',*,*,#5814,.T.);
#7543=ORIENTED_EDGE('',*,*,#5760,.F.);
#7544=ORIENTED_EDGE('',*,*,#5818,.F.);
#7545=ORIENTED_EDGE('',*,*,#5819,.T.);
#7546=ORIENTED_EDGE('',*,*,#5816,.T.);
#7547=ORIENTED_EDGE('',*,*,#5759,.F.);
#7548=ORIENTED_EDGE('',*,*,#5811,.F.);
#7549=ORIENTED_EDGE('',*,*,#5820,.T.);
#7550=ORIENTED_EDGE('',*,*,#5818,.T.);
#7551=ORIENTED_EDGE('',*,*,#5810,.F.);
#7552=ORIENTED_EDGE('',*,*,#5813,.F.);
#7553=ORIENTED_EDGE('',*,*,#5815,.F.);
#7554=ORIENTED_EDGE('',*,*,#5817,.F.);
#7555=ORIENTED_EDGE('',*,*,#5819,.F.);
#7556=ORIENTED_EDGE('',*,*,#5820,.F.);
#7557=ORIENTED_EDGE('',*,*,#5708,.T.);
#7558=ORIENTED_EDGE('',*,*,#5795,.T.);
#7559=ORIENTED_EDGE('',*,*,#5793,.T.);
#7560=ORIENTED_EDGE('',*,*,#5751,.T.);
#7561=ORIENTED_EDGE('',*,*,#5821,.F.);
#7562=ORIENTED_EDGE('',*,*,#5757,.T.);
#7563=ORIENTED_EDGE('',*,*,#5777,.T.);
#7564=ORIENTED_EDGE('',*,*,#5794,.F.);
#7565=ORIENTED_EDGE('',*,*,#5822,.F.);
#7566=ORIENTED_EDGE('',*,*,#5758,.T.);
#7567=ORIENTED_EDGE('',*,*,#5822,.T.);
#7568=ORIENTED_EDGE('',*,*,#5796,.T.);
#7569=ORIENTED_EDGE('',*,*,#5821,.T.);
#7570=ORIENTED_EDGE('',*,*,#5742,.F.);
#7571=ORIENTED_EDGE('',*,*,#5823,.F.);
#7572=ORIENTED_EDGE('',*,*,#5784,.F.);
#7573=ORIENTED_EDGE('',*,*,#5824,.F.);
#7574=ORIENTED_EDGE('',*,*,#5721,.T.);
#7575=ORIENTED_EDGE('',*,*,#5715,.T.);
#7576=ORIENTED_EDGE('',*,*,#5743,.F.);
#7577=ORIENTED_EDGE('',*,*,#5733,.F.);
#7578=ORIENTED_EDGE('',*,*,#5824,.T.);
#7579=ORIENTED_EDGE('',*,*,#5783,.T.);
#7580=ORIENTED_EDGE('',*,*,#5747,.F.);
#7581=ORIENTED_EDGE('',*,*,#5785,.F.);
#7582=ORIENTED_EDGE('',*,*,#5823,.T.);
#7583=ORIENTED_EDGE('',*,*,#5741,.T.);
#7584=ORIENTED_EDGE('',*,*,#5825,.T.);
#7585=ORIENTED_EDGE('',*,*,#5826,.T.);
#7586=ORIENTED_EDGE('',*,*,#5827,.F.);
#7587=ORIENTED_EDGE('',*,*,#5828,.F.);
#7588=ORIENTED_EDGE('',*,*,#5829,.F.);
#7589=ORIENTED_EDGE('',*,*,#5826,.F.);
#7590=ORIENTED_EDGE('',*,*,#5830,.F.);
#7591=ORIENTED_EDGE('',*,*,#5831,.T.);
#7592=ORIENTED_EDGE('',*,*,#5832,.F.);
#7593=ORIENTED_EDGE('',*,*,#5831,.F.);
#7594=ORIENTED_EDGE('',*,*,#5833,.T.);
#7595=ORIENTED_EDGE('',*,*,#5834,.T.);
#7596=ORIENTED_EDGE('',*,*,#5835,.F.);
#7597=ORIENTED_EDGE('',*,*,#5834,.F.);
#7598=ORIENTED_EDGE('',*,*,#5836,.F.);
#7599=ORIENTED_EDGE('',*,*,#5837,.T.);
#7600=ORIENTED_EDGE('',*,*,#5838,.F.);
#7601=ORIENTED_EDGE('',*,*,#5837,.F.);
#7602=ORIENTED_EDGE('',*,*,#5839,.T.);
#7603=ORIENTED_EDGE('',*,*,#5840,.T.);
#7604=ORIENTED_EDGE('',*,*,#5841,.F.);
#7605=ORIENTED_EDGE('',*,*,#5840,.F.);
#7606=ORIENTED_EDGE('',*,*,#5842,.T.);
#7607=ORIENTED_EDGE('',*,*,#5843,.T.);
#7608=ORIENTED_EDGE('',*,*,#5844,.F.);
#7609=ORIENTED_EDGE('',*,*,#5843,.F.);
#7610=ORIENTED_EDGE('',*,*,#5845,.T.);
#7611=ORIENTED_EDGE('',*,*,#5846,.T.);
#7612=ORIENTED_EDGE('',*,*,#5847,.F.);
#7613=ORIENTED_EDGE('',*,*,#5846,.F.);
#7614=ORIENTED_EDGE('',*,*,#5848,.T.);
#7615=ORIENTED_EDGE('',*,*,#5849,.T.);
#7616=ORIENTED_EDGE('',*,*,#5850,.F.);
#7617=ORIENTED_EDGE('',*,*,#5851,.F.);
#7618=ORIENTED_EDGE('',*,*,#5852,.F.);
#7619=ORIENTED_EDGE('',*,*,#5853,.T.);
#7620=ORIENTED_EDGE('',*,*,#5854,.F.);
#7621=ORIENTED_EDGE('',*,*,#5855,.F.);
#7622=ORIENTED_EDGE('',*,*,#5856,.T.);
#7623=ORIENTED_EDGE('',*,*,#5857,.T.);
#7624=ORIENTED_EDGE('',*,*,#5858,.F.);
#7625=ORIENTED_EDGE('',*,*,#5859,.T.);
#7626=ORIENTED_EDGE('',*,*,#5860,.T.);
#7627=ORIENTED_EDGE('',*,*,#5857,.F.);
#7628=ORIENTED_EDGE('',*,*,#5861,.T.);
#7629=ORIENTED_EDGE('',*,*,#5862,.T.);
#7630=ORIENTED_EDGE('',*,*,#5863,.F.);
#7631=ORIENTED_EDGE('',*,*,#5849,.F.);
#7632=ORIENTED_EDGE('',*,*,#5864,.T.);
#7633=ORIENTED_EDGE('',*,*,#5861,.F.);
#7634=ORIENTED_EDGE('',*,*,#5865,.F.);
#7635=ORIENTED_EDGE('',*,*,#5866,.F.);
#7636=ORIENTED_EDGE('',*,*,#5867,.T.);
#7637=ORIENTED_EDGE('',*,*,#5868,.F.);
#7638=ORIENTED_EDGE('',*,*,#5867,.F.);
#7639=ORIENTED_EDGE('',*,*,#5869,.T.);
#7640=ORIENTED_EDGE('',*,*,#5870,.T.);
#7641=ORIENTED_EDGE('',*,*,#5863,.T.);
#7642=ORIENTED_EDGE('',*,*,#5871,.T.);
#7643=ORIENTED_EDGE('',*,*,#5870,.F.);
#7644=ORIENTED_EDGE('',*,*,#5872,.F.);
#7645=ORIENTED_EDGE('',*,*,#5873,.F.);
#7646=ORIENTED_EDGE('',*,*,#5850,.T.);
#7647=ORIENTED_EDGE('',*,*,#5874,.F.);
#7648=ORIENTED_EDGE('',*,*,#5875,.T.);
#7649=ORIENTED_EDGE('',*,*,#5876,.F.);
#7650=ORIENTED_EDGE('',*,*,#5877,.F.);
#7651=ORIENTED_EDGE('',*,*,#5878,.T.);
#7652=ORIENTED_EDGE('',*,*,#5879,.F.);
#7653=ORIENTED_EDGE('',*,*,#5880,.T.);
#7654=ORIENTED_EDGE('',*,*,#5881,.T.);
#7655=ORIENTED_EDGE('',*,*,#5882,.F.);
#7656=ORIENTED_EDGE('',*,*,#5854,.T.);
#7657=ORIENTED_EDGE('',*,*,#5883,.F.);
#7658=ORIENTED_EDGE('',*,*,#5884,.T.);
#7659=ORIENTED_EDGE('',*,*,#5885,.T.);
#7660=ORIENTED_EDGE('',*,*,#5852,.T.);
#7661=ORIENTED_EDGE('',*,*,#5886,.F.);
#7662=ORIENTED_EDGE('',*,*,#5887,.T.);
#7663=ORIENTED_EDGE('',*,*,#5865,.T.);
#7664=ORIENTED_EDGE('',*,*,#5856,.F.);
#7665=ORIENTED_EDGE('',*,*,#5888,.T.);
#7666=ORIENTED_EDGE('',*,*,#5875,.F.);
#7667=ORIENTED_EDGE('',*,*,#5889,.F.);
#7668=ORIENTED_EDGE('',*,*,#5872,.T.);
#7669=ORIENTED_EDGE('',*,*,#5869,.F.);
#7670=ORIENTED_EDGE('',*,*,#5866,.T.);
#7671=ORIENTED_EDGE('',*,*,#5887,.F.);
#7672=ORIENTED_EDGE('',*,*,#5890,.F.);
#7673=ORIENTED_EDGE('',*,*,#5881,.F.);
#7674=ORIENTED_EDGE('',*,*,#5891,.T.);
#7675=ORIENTED_EDGE('',*,*,#5892,.F.);
#7676=ORIENTED_EDGE('',*,*,#5828,.T.);
#7677=ORIENTED_EDGE('',*,*,#5893,.F.);
#7678=ORIENTED_EDGE('',*,*,#5835,.T.);
#7679=ORIENTED_EDGE('',*,*,#5839,.F.);
#7680=ORIENTED_EDGE('',*,*,#5864,.F.);
#7681=ORIENTED_EDGE('',*,*,#5868,.T.);
#7682=ORIENTED_EDGE('',*,*,#5871,.F.);
#7683=ORIENTED_EDGE('',*,*,#5862,.F.);
#7684=ORIENTED_EDGE('',*,*,#5847,.T.);
#7685=ORIENTED_EDGE('',*,*,#5845,.F.);
#7686=ORIENTED_EDGE('',*,*,#5844,.T.);
#7687=ORIENTED_EDGE('',*,*,#5842,.F.);
#7688=ORIENTED_EDGE('',*,*,#5841,.T.);
#7689=ORIENTED_EDGE('',*,*,#5855,.T.);
#7690=ORIENTED_EDGE('',*,*,#5882,.T.);
#7691=ORIENTED_EDGE('',*,*,#5890,.T.);
#7692=ORIENTED_EDGE('',*,*,#5886,.T.);
#7693=ORIENTED_EDGE('',*,*,#5851,.T.);
#7694=ORIENTED_EDGE('',*,*,#5873,.T.);
#7695=ORIENTED_EDGE('',*,*,#5889,.T.);
#7696=ORIENTED_EDGE('',*,*,#5874,.T.);
#7697=ORIENTED_EDGE('',*,*,#5833,.F.);
#7698=ORIENTED_EDGE('',*,*,#5838,.T.);
#7699=ORIENTED_EDGE('',*,*,#5825,.F.);
#7700=ORIENTED_EDGE('',*,*,#5832,.T.);
#7701=ORIENTED_EDGE('',*,*,#5894,.T.);
#7702=ORIENTED_EDGE('',*,*,#5895,.F.);
#7703=ORIENTED_EDGE('',*,*,#5891,.F.);
#7704=ORIENTED_EDGE('',*,*,#5880,.F.);
#7705=ORIENTED_EDGE('',*,*,#5896,.F.);
#7706=ORIENTED_EDGE('',*,*,#5894,.F.);
#7707=ORIENTED_EDGE('',*,*,#5897,.F.);
#7708=ORIENTED_EDGE('',*,*,#5898,.T.);
#7709=ORIENTED_EDGE('',*,*,#5899,.F.);
#7710=ORIENTED_EDGE('',*,*,#5900,.T.);
#7711=ORIENTED_EDGE('',*,*,#5901,.F.);
#7712=ORIENTED_EDGE('',*,*,#5876,.T.);
#7713=ORIENTED_EDGE('',*,*,#5888,.F.);
#7714=ORIENTED_EDGE('',*,*,#5902,.F.);
#7715=ORIENTED_EDGE('',*,*,#5900,.F.);
#7716=ORIENTED_EDGE('',*,*,#5903,.F.);
#7717=ORIENTED_EDGE('',*,*,#5898,.F.);
#7718=ORIENTED_EDGE('',*,*,#5904,.F.);
#7719=ORIENTED_EDGE('',*,*,#5878,.F.);
#7720=ORIENTED_EDGE('',*,*,#5905,.F.);
#7721=ORIENTED_EDGE('',*,*,#5899,.T.);
#7722=ORIENTED_EDGE('',*,*,#5905,.T.);
#7723=ORIENTED_EDGE('',*,*,#5877,.T.);
#7724=ORIENTED_EDGE('',*,*,#5903,.T.);
#7725=ORIENTED_EDGE('',*,*,#5879,.T.);
#7726=ORIENTED_EDGE('',*,*,#5904,.T.);
#7727=ORIENTED_EDGE('',*,*,#5897,.T.);
#7728=ORIENTED_EDGE('',*,*,#5896,.T.);
#7729=ORIENTED_EDGE('',*,*,#5827,.T.);
#7730=ORIENTED_EDGE('',*,*,#5829,.T.);
#7731=ORIENTED_EDGE('',*,*,#5892,.T.);
#7732=ORIENTED_EDGE('',*,*,#5895,.T.);
#7733=ORIENTED_EDGE('',*,*,#5901,.T.);
#7734=ORIENTED_EDGE('',*,*,#5902,.T.);
#7735=ORIENTED_EDGE('',*,*,#5893,.T.);
#7736=ORIENTED_EDGE('',*,*,#5884,.F.);
#7737=ORIENTED_EDGE('',*,*,#5906,.F.);
#7738=ORIENTED_EDGE('',*,*,#5859,.F.);
#7739=ORIENTED_EDGE('',*,*,#5907,.F.);
#7740=ORIENTED_EDGE('',*,*,#5830,.T.);
#7741=ORIENTED_EDGE('',*,*,#5836,.T.);
#7742=ORIENTED_EDGE('',*,*,#5848,.F.);
#7743=ORIENTED_EDGE('',*,*,#5885,.F.);
#7744=ORIENTED_EDGE('',*,*,#5907,.T.);
#7745=ORIENTED_EDGE('',*,*,#5858,.T.);
#7746=ORIENTED_EDGE('',*,*,#5853,.F.);
#7747=ORIENTED_EDGE('',*,*,#5860,.F.);
#7748=ORIENTED_EDGE('',*,*,#5906,.T.);
#7749=ORIENTED_EDGE('',*,*,#5883,.T.);
#7750=ORIENTED_EDGE('',*,*,#5908,.F.);
#7751=ORIENTED_EDGE('',*,*,#5909,.T.);
#7752=ORIENTED_EDGE('',*,*,#5910,.T.);
#7753=ORIENTED_EDGE('',*,*,#5911,.T.);
#7754=ORIENTED_EDGE('',*,*,#5912,.T.);
#7755=ORIENTED_EDGE('',*,*,#5909,.F.);
#7756=ORIENTED_EDGE('',*,*,#5913,.T.);
#7757=ORIENTED_EDGE('',*,*,#5914,.T.);
#7758=ORIENTED_EDGE('',*,*,#5915,.T.);
#7759=ORIENTED_EDGE('',*,*,#5914,.F.);
#7760=ORIENTED_EDGE('',*,*,#5916,.F.);
#7761=ORIENTED_EDGE('',*,*,#5917,.T.);
#7762=ORIENTED_EDGE('',*,*,#5918,.T.);
#7763=ORIENTED_EDGE('',*,*,#5917,.F.);
#7764=ORIENTED_EDGE('',*,*,#5919,.T.);
#7765=ORIENTED_EDGE('',*,*,#5920,.T.);
#7766=ORIENTED_EDGE('',*,*,#5921,.T.);
#7767=ORIENTED_EDGE('',*,*,#5920,.F.);
#7768=ORIENTED_EDGE('',*,*,#5922,.F.);
#7769=ORIENTED_EDGE('',*,*,#5923,.T.);
#7770=ORIENTED_EDGE('',*,*,#5924,.T.);
#7771=ORIENTED_EDGE('',*,*,#5923,.F.);
#7772=ORIENTED_EDGE('',*,*,#5925,.F.);
#7773=ORIENTED_EDGE('',*,*,#5926,.T.);
#7774=ORIENTED_EDGE('',*,*,#5927,.T.);
#7775=ORIENTED_EDGE('',*,*,#5926,.F.);
#7776=ORIENTED_EDGE('',*,*,#5928,.F.);
#7777=ORIENTED_EDGE('',*,*,#5929,.T.);
#7778=ORIENTED_EDGE('',*,*,#5930,.T.);
#7779=ORIENTED_EDGE('',*,*,#5929,.F.);
#7780=ORIENTED_EDGE('',*,*,#5931,.F.);
#7781=ORIENTED_EDGE('',*,*,#5932,.T.);
#7782=ORIENTED_EDGE('',*,*,#5933,.T.);
#7783=ORIENTED_EDGE('',*,*,#5934,.T.);
#7784=ORIENTED_EDGE('',*,*,#5935,.F.);
#7785=ORIENTED_EDGE('',*,*,#5936,.F.);
#7786=ORIENTED_EDGE('',*,*,#5937,.F.);
#7787=ORIENTED_EDGE('',*,*,#5938,.F.);
#7788=ORIENTED_EDGE('',*,*,#5939,.T.);
#7789=ORIENTED_EDGE('',*,*,#5940,.T.);
#7790=ORIENTED_EDGE('',*,*,#5941,.T.);
#7791=ORIENTED_EDGE('',*,*,#5935,.T.);
#7792=ORIENTED_EDGE('',*,*,#5942,.T.);
#7793=ORIENTED_EDGE('',*,*,#5943,.F.);
#7794=ORIENTED_EDGE('',*,*,#5944,.F.);
#7795=ORIENTED_EDGE('',*,*,#5937,.T.);
#7796=ORIENTED_EDGE('',*,*,#5945,.F.);
#7797=ORIENTED_EDGE('',*,*,#5946,.F.);
#7798=ORIENTED_EDGE('',*,*,#5947,.F.);
#7799=ORIENTED_EDGE('',*,*,#5948,.F.);
#7800=ORIENTED_EDGE('',*,*,#5949,.T.);
#7801=ORIENTED_EDGE('',*,*,#5950,.T.);
#7802=ORIENTED_EDGE('',*,*,#5944,.T.);
#7803=ORIENTED_EDGE('',*,*,#5951,.T.);
#7804=ORIENTED_EDGE('',*,*,#5952,.F.);
#7805=ORIENTED_EDGE('',*,*,#5953,.F.);
#7806=ORIENTED_EDGE('',*,*,#5948,.T.);
#7807=ORIENTED_EDGE('',*,*,#5942,.F.);
#7808=ORIENTED_EDGE('',*,*,#5934,.F.);
#7809=ORIENTED_EDGE('',*,*,#5954,.T.);
#7810=ORIENTED_EDGE('',*,*,#5955,.T.);
#7811=ORIENTED_EDGE('',*,*,#5952,.T.);
#7812=ORIENTED_EDGE('',*,*,#5956,.F.);
#7813=ORIENTED_EDGE('',*,*,#5957,.T.);
#7814=ORIENTED_EDGE('',*,*,#5932,.F.);
#7815=ORIENTED_EDGE('',*,*,#5958,.F.);
#7816=ORIENTED_EDGE('',*,*,#5959,.F.);
#7817=ORIENTED_EDGE('',*,*,#5960,.T.);
#7818=ORIENTED_EDGE('',*,*,#5940,.F.);
#7819=ORIENTED_EDGE('',*,*,#5961,.T.);
#7820=ORIENTED_EDGE('',*,*,#5962,.F.);
#7821=ORIENTED_EDGE('',*,*,#5963,.F.);
#7822=ORIENTED_EDGE('',*,*,#5964,.T.);
#7823=ORIENTED_EDGE('',*,*,#5965,.F.);
#7824=ORIENTED_EDGE('',*,*,#5966,.T.);
#7825=ORIENTED_EDGE('',*,*,#5967,.T.);
#7826=ORIENTED_EDGE('',*,*,#5968,.F.);
#7827=ORIENTED_EDGE('',*,*,#5969,.T.);
#7828=ORIENTED_EDGE('',*,*,#5938,.T.);
#7829=ORIENTED_EDGE('',*,*,#5950,.F.);
#7830=ORIENTED_EDGE('',*,*,#5970,.F.);
#7831=ORIENTED_EDGE('',*,*,#5971,.F.);
#7832=ORIENTED_EDGE('',*,*,#5972,.T.);
#7833=ORIENTED_EDGE('',*,*,#5911,.F.);
#7834=ORIENTED_EDGE('',*,*,#5973,.T.);
#7835=ORIENTED_EDGE('',*,*,#5974,.F.);
#7836=ORIENTED_EDGE('',*,*,#5962,.T.);
#7837=ORIENTED_EDGE('',*,*,#5975,.T.);
#7838=ORIENTED_EDGE('',*,*,#5970,.T.);
#7839=ORIENTED_EDGE('',*,*,#5949,.F.);
#7840=ORIENTED_EDGE('',*,*,#5953,.T.);
#7841=ORIENTED_EDGE('',*,*,#5955,.F.);
#7842=ORIENTED_EDGE('',*,*,#5976,.T.);
#7843=ORIENTED_EDGE('',*,*,#5968,.T.);
#7844=ORIENTED_EDGE('',*,*,#5918,.F.);
#7845=ORIENTED_EDGE('',*,*,#5922,.T.);
#7846=ORIENTED_EDGE('',*,*,#5947,.T.);
#7847=ORIENTED_EDGE('',*,*,#5943,.T.);
#7848=ORIENTED_EDGE('',*,*,#5956,.T.);
#7849=ORIENTED_EDGE('',*,*,#5951,.F.);
#7850=ORIENTED_EDGE('',*,*,#5930,.F.);
#7851=ORIENTED_EDGE('',*,*,#5928,.T.);
#7852=ORIENTED_EDGE('',*,*,#5927,.F.);
#7853=ORIENTED_EDGE('',*,*,#5925,.T.);
#7854=ORIENTED_EDGE('',*,*,#5924,.F.);
#7855=ORIENTED_EDGE('',*,*,#5939,.F.);
#7856=ORIENTED_EDGE('',*,*,#5969,.F.);
#7857=ORIENTED_EDGE('',*,*,#5975,.F.);
#7858=ORIENTED_EDGE('',*,*,#5961,.F.);
#7859=ORIENTED_EDGE('',*,*,#5933,.F.);
#7860=ORIENTED_EDGE('',*,*,#5957,.F.);
#7861=ORIENTED_EDGE('',*,*,#5976,.F.);
#7862=ORIENTED_EDGE('',*,*,#5954,.F.);
#7863=ORIENTED_EDGE('',*,*,#5916,.T.);
#7864=ORIENTED_EDGE('',*,*,#5921,.F.);
#7865=ORIENTED_EDGE('',*,*,#5908,.T.);
#7866=ORIENTED_EDGE('',*,*,#5915,.F.);
#7867=ORIENTED_EDGE('',*,*,#5977,.F.);
#7868=ORIENTED_EDGE('',*,*,#5978,.T.);
#7869=ORIENTED_EDGE('',*,*,#5963,.T.);
#7870=ORIENTED_EDGE('',*,*,#5974,.T.);
#7871=ORIENTED_EDGE('',*,*,#5979,.T.);
#7872=ORIENTED_EDGE('',*,*,#5977,.T.);
#7873=ORIENTED_EDGE('',*,*,#5980,.T.);
#7874=ORIENTED_EDGE('',*,*,#5981,.F.);
#7875=ORIENTED_EDGE('',*,*,#5982,.T.);
#7876=ORIENTED_EDGE('',*,*,#5983,.F.);
#7877=ORIENTED_EDGE('',*,*,#5984,.T.);
#7878=ORIENTED_EDGE('',*,*,#5967,.F.);
#7879=ORIENTED_EDGE('',*,*,#5985,.T.);
#7880=ORIENTED_EDGE('',*,*,#5981,.T.);
#7881=ORIENTED_EDGE('',*,*,#5986,.T.);
#7882=ORIENTED_EDGE('',*,*,#5971,.T.);
#7883=ORIENTED_EDGE('',*,*,#5983,.T.);
#7884=ORIENTED_EDGE('',*,*,#5987,.T.);
#7885=ORIENTED_EDGE('',*,*,#5965,.T.);
#7886=ORIENTED_EDGE('',*,*,#5988,.T.);
#7887=ORIENTED_EDGE('',*,*,#5982,.F.);
#7888=ORIENTED_EDGE('',*,*,#5985,.F.);
#7889=ORIENTED_EDGE('',*,*,#5966,.F.);
#7890=ORIENTED_EDGE('',*,*,#5987,.F.);
#7891=ORIENTED_EDGE('',*,*,#5964,.F.);
#7892=ORIENTED_EDGE('',*,*,#5978,.F.);
#7893=ORIENTED_EDGE('',*,*,#5984,.F.);
#7894=ORIENTED_EDGE('',*,*,#5988,.F.);
#7895=ORIENTED_EDGE('',*,*,#5912,.F.);
#7896=ORIENTED_EDGE('',*,*,#5972,.F.);
#7897=ORIENTED_EDGE('',*,*,#5986,.F.);
#7898=ORIENTED_EDGE('',*,*,#5980,.F.);
#7899=ORIENTED_EDGE('',*,*,#5979,.F.);
#7900=ORIENTED_EDGE('',*,*,#5973,.F.);
#7901=ORIENTED_EDGE('',*,*,#5910,.F.);
#7902=ORIENTED_EDGE('',*,*,#5959,.T.);
#7903=ORIENTED_EDGE('',*,*,#5989,.T.);
#7904=ORIENTED_EDGE('',*,*,#5946,.T.);
#7905=ORIENTED_EDGE('',*,*,#5990,.T.);
#7906=ORIENTED_EDGE('',*,*,#5913,.F.);
#7907=ORIENTED_EDGE('',*,*,#5919,.F.);
#7908=ORIENTED_EDGE('',*,*,#5931,.T.);
#7909=ORIENTED_EDGE('',*,*,#5941,.F.);
#7910=ORIENTED_EDGE('',*,*,#5989,.F.);
#7911=ORIENTED_EDGE('',*,*,#5958,.T.);
#7912=ORIENTED_EDGE('',*,*,#5936,.T.);
#7913=ORIENTED_EDGE('',*,*,#5960,.F.);
#7914=ORIENTED_EDGE('',*,*,#5990,.F.);
#7915=ORIENTED_EDGE('',*,*,#5945,.T.);
#7916=ORIENTED_EDGE('',*,*,#5991,.F.);
#7917=ORIENTED_EDGE('',*,*,#5992,.T.);
#7918=ORIENTED_EDGE('',*,*,#5993,.T.);
#7919=ORIENTED_EDGE('',*,*,#5992,.F.);
#7920=ORIENTED_EDGE('',*,*,#5994,.F.);
#7921=ORIENTED_EDGE('',*,*,#5995,.T.);
#7922=ORIENTED_EDGE('',*,*,#5996,.T.);
#7923=ORIENTED_EDGE('',*,*,#5995,.F.);
#7924=ORIENTED_EDGE('',*,*,#5997,.F.);
#7925=ORIENTED_EDGE('',*,*,#5998,.T.);
#7926=ORIENTED_EDGE('',*,*,#5999,.T.);
#7927=ORIENTED_EDGE('',*,*,#5998,.F.);
#7928=ORIENTED_EDGE('',*,*,#6000,.F.);
#7929=ORIENTED_EDGE('',*,*,#6001,.T.);
#7930=ORIENTED_EDGE('',*,*,#6002,.T.);
#7931=ORIENTED_EDGE('',*,*,#6001,.F.);
#7932=ORIENTED_EDGE('',*,*,#6003,.F.);
#7933=ORIENTED_EDGE('',*,*,#6004,.T.);
#7934=ORIENTED_EDGE('',*,*,#6005,.F.);
#7935=ORIENTED_EDGE('',*,*,#6004,.F.);
#7936=ORIENTED_EDGE('',*,*,#6006,.F.);
#7937=ORIENTED_EDGE('',*,*,#6007,.T.);
#7938=ORIENTED_EDGE('',*,*,#6008,.T.);
#7939=ORIENTED_EDGE('',*,*,#6007,.F.);
#7940=ORIENTED_EDGE('',*,*,#6009,.F.);
#7941=ORIENTED_EDGE('',*,*,#6010,.T.);
#7942=ORIENTED_EDGE('',*,*,#6011,.T.);
#7943=ORIENTED_EDGE('',*,*,#6010,.F.);
#7944=ORIENTED_EDGE('',*,*,#6012,.F.);
#7945=ORIENTED_EDGE('',*,*,#6013,.T.);
#7946=ORIENTED_EDGE('',*,*,#6014,.T.);
#7947=ORIENTED_EDGE('',*,*,#6013,.F.);
#7948=ORIENTED_EDGE('',*,*,#6015,.F.);
#7949=ORIENTED_EDGE('',*,*,#6016,.T.);
#7950=ORIENTED_EDGE('',*,*,#6017,.T.);
#7951=ORIENTED_EDGE('',*,*,#6016,.F.);
#7952=ORIENTED_EDGE('',*,*,#6018,.F.);
#7953=ORIENTED_EDGE('',*,*,#6019,.T.);
#7954=ORIENTED_EDGE('',*,*,#6020,.T.);
#7955=ORIENTED_EDGE('',*,*,#6019,.F.);
#7956=ORIENTED_EDGE('',*,*,#6021,.F.);
#7957=ORIENTED_EDGE('',*,*,#6022,.T.);
#7958=ORIENTED_EDGE('',*,*,#6023,.F.);
#7959=ORIENTED_EDGE('',*,*,#6024,.T.);
#7960=ORIENTED_EDGE('',*,*,#6025,.F.);
#7961=ORIENTED_EDGE('',*,*,#6026,.T.);
#7962=ORIENTED_EDGE('',*,*,#6027,.F.);
#7963=ORIENTED_EDGE('',*,*,#6028,.T.);
#7964=ORIENTED_EDGE('',*,*,#6029,.F.);
#7965=ORIENTED_EDGE('',*,*,#6030,.T.);
#7966=ORIENTED_EDGE('',*,*,#6031,.F.);
#7967=ORIENTED_EDGE('',*,*,#6032,.T.);
#7968=ORIENTED_EDGE('',*,*,#6026,.F.);
#7969=ORIENTED_EDGE('',*,*,#6033,.F.);
#7970=ORIENTED_EDGE('',*,*,#6032,.F.);
#7971=ORIENTED_EDGE('',*,*,#6034,.F.);
#7972=ORIENTED_EDGE('',*,*,#6022,.F.);
#7973=ORIENTED_EDGE('',*,*,#6035,.F.);
#7974=ORIENTED_EDGE('',*,*,#6028,.F.);
#7975=ORIENTED_EDGE('',*,*,#6036,.F.);
#7976=ORIENTED_EDGE('',*,*,#6037,.F.);
#7977=ORIENTED_EDGE('',*,*,#6038,.T.);
#7978=ORIENTED_EDGE('',*,*,#6039,.T.);
#7979=ORIENTED_EDGE('',*,*,#6040,.F.);
#7980=ORIENTED_EDGE('',*,*,#6041,.F.);
#7981=ORIENTED_EDGE('',*,*,#6042,.T.);
#7982=ORIENTED_EDGE('',*,*,#6043,.T.);
#7983=ORIENTED_EDGE('',*,*,#6039,.F.);
#7984=ORIENTED_EDGE('',*,*,#6042,.F.);
#7985=ORIENTED_EDGE('',*,*,#6044,.T.);
#7986=ORIENTED_EDGE('',*,*,#6045,.T.);
#7987=ORIENTED_EDGE('',*,*,#6046,.F.);
#7988=ORIENTED_EDGE('',*,*,#6047,.F.);
#7989=ORIENTED_EDGE('',*,*,#6048,.T.);
#7990=ORIENTED_EDGE('',*,*,#6049,.T.);
#7991=ORIENTED_EDGE('',*,*,#6045,.F.);
#7992=ORIENTED_EDGE('',*,*,#6050,.F.);
#7993=ORIENTED_EDGE('',*,*,#6051,.T.);
#7994=ORIENTED_EDGE('',*,*,#6052,.T.);
#7995=ORIENTED_EDGE('',*,*,#6048,.F.);
#7996=ORIENTED_EDGE('',*,*,#6053,.F.);
#7997=ORIENTED_EDGE('',*,*,#6054,.T.);
#7998=ORIENTED_EDGE('',*,*,#6055,.T.);
#7999=ORIENTED_EDGE('',*,*,#6051,.F.);
#8000=ORIENTED_EDGE('',*,*,#6056,.F.);
#8001=ORIENTED_EDGE('',*,*,#6057,.T.);
#8002=ORIENTED_EDGE('',*,*,#6058,.T.);
#8003=ORIENTED_EDGE('',*,*,#6054,.F.);
#8004=ORIENTED_EDGE('',*,*,#6059,.F.);
#8005=ORIENTED_EDGE('',*,*,#6037,.T.);
#8006=ORIENTED_EDGE('',*,*,#6060,.T.);
#8007=ORIENTED_EDGE('',*,*,#6057,.F.);
#8008=ORIENTED_EDGE('',*,*,#6061,.T.);
#8009=ORIENTED_EDGE('',*,*,#6062,.F.);
#8010=ORIENTED_EDGE('',*,*,#6063,.T.);
#8011=ORIENTED_EDGE('',*,*,#6064,.F.);
#8012=ORIENTED_EDGE('',*,*,#6065,.T.);
#8013=ORIENTED_EDGE('',*,*,#6066,.F.);
#8014=ORIENTED_EDGE('',*,*,#6067,.T.);
#8015=ORIENTED_EDGE('',*,*,#6068,.F.);
#8016=ORIENTED_EDGE('',*,*,#6069,.T.);
#8017=ORIENTED_EDGE('',*,*,#6070,.F.);
#8018=ORIENTED_EDGE('',*,*,#6071,.T.);
#8019=ORIENTED_EDGE('',*,*,#6072,.F.);
#8020=ORIENTED_EDGE('',*,*,#6073,.T.);
#8021=ORIENTED_EDGE('',*,*,#6074,.F.);
#8022=ORIENTED_EDGE('',*,*,#6075,.T.);
#8023=ORIENTED_EDGE('',*,*,#6076,.F.);
#8024=ORIENTED_EDGE('',*,*,#6077,.T.);
#8025=ORIENTED_EDGE('',*,*,#6078,.F.);
#8026=ORIENTED_EDGE('',*,*,#6079,.T.);
#8027=ORIENTED_EDGE('',*,*,#6080,.F.);
#8028=ORIENTED_EDGE('',*,*,#6079,.F.);
#8029=ORIENTED_EDGE('',*,*,#6081,.F.);
#8030=ORIENTED_EDGE('',*,*,#6024,.F.);
#8031=ORIENTED_EDGE('',*,*,#6082,.F.);
#8032=ORIENTED_EDGE('',*,*,#6083,.F.);
#8033=ORIENTED_EDGE('',*,*,#6077,.F.);
#8034=ORIENTED_EDGE('',*,*,#6084,.F.);
#8035=ORIENTED_EDGE('',*,*,#6075,.F.);
#8036=ORIENTED_EDGE('',*,*,#6071,.F.);
#8037=ORIENTED_EDGE('',*,*,#6085,.F.);
#8038=ORIENTED_EDGE('',*,*,#6073,.F.);
#8039=ORIENTED_EDGE('',*,*,#6086,.F.);
#8040=ORIENTED_EDGE('',*,*,#6063,.F.);
#8041=ORIENTED_EDGE('',*,*,#6087,.F.);
#8042=ORIENTED_EDGE('',*,*,#6069,.F.);
#8043=ORIENTED_EDGE('',*,*,#6088,.F.);
#8044=ORIENTED_EDGE('',*,*,#6067,.F.);
#8045=ORIENTED_EDGE('',*,*,#6089,.F.);
#8046=ORIENTED_EDGE('',*,*,#6061,.F.);
#8047=ORIENTED_EDGE('',*,*,#6090,.F.);
#8048=ORIENTED_EDGE('',*,*,#6091,.F.);
#8049=ORIENTED_EDGE('',*,*,#6065,.F.);
#8050=ORIENTED_EDGE('',*,*,#6092,.F.);
#8051=ORIENTED_EDGE('',*,*,#6030,.F.);
#8052=ORIENTED_EDGE('',*,*,#6080,.T.);
#8053=ORIENTED_EDGE('',*,*,#6082,.T.);
#8054=ORIENTED_EDGE('',*,*,#6023,.T.);
#8055=ORIENTED_EDGE('',*,*,#6036,.T.);
#8056=ORIENTED_EDGE('',*,*,#6027,.T.);
#8057=ORIENTED_EDGE('',*,*,#6034,.T.);
#8058=ORIENTED_EDGE('',*,*,#6031,.T.);
#8059=ORIENTED_EDGE('',*,*,#6092,.T.);
#8060=ORIENTED_EDGE('',*,*,#6068,.T.);
#8061=ORIENTED_EDGE('',*,*,#6090,.T.);
#8062=ORIENTED_EDGE('',*,*,#6064,.T.);
#8063=ORIENTED_EDGE('',*,*,#6088,.T.);
#8064=ORIENTED_EDGE('',*,*,#6072,.T.);
#8065=ORIENTED_EDGE('',*,*,#6086,.T.);
#8066=ORIENTED_EDGE('',*,*,#6076,.T.);
#8067=ORIENTED_EDGE('',*,*,#6084,.T.);
#8068=ORIENTED_EDGE('',*,*,#6060,.F.);
#8069=ORIENTED_EDGE('',*,*,#6040,.T.);
#8070=ORIENTED_EDGE('',*,*,#6043,.F.);
#8071=ORIENTED_EDGE('',*,*,#6046,.T.);
#8072=ORIENTED_EDGE('',*,*,#6049,.F.);
#8073=ORIENTED_EDGE('',*,*,#6052,.F.);
#8074=ORIENTED_EDGE('',*,*,#6055,.F.);
#8075=ORIENTED_EDGE('',*,*,#6058,.F.);
#8076=ORIENTED_EDGE('',*,*,#5993,.F.);
#8077=ORIENTED_EDGE('',*,*,#5996,.F.);
#8078=ORIENTED_EDGE('',*,*,#6003,.T.);
#8079=ORIENTED_EDGE('',*,*,#6014,.F.);
#8080=ORIENTED_EDGE('',*,*,#5999,.F.);
#8081=ORIENTED_EDGE('',*,*,#6002,.F.);
#8082=ORIENTED_EDGE('',*,*,#6000,.T.);
#8083=ORIENTED_EDGE('',*,*,#6020,.F.);
#8084=ORIENTED_EDGE('',*,*,#5997,.T.);
#8085=ORIENTED_EDGE('',*,*,#6017,.F.);
#8086=ORIENTED_EDGE('',*,*,#6035,.T.);
#8087=ORIENTED_EDGE('',*,*,#6021,.T.);
#8088=ORIENTED_EDGE('',*,*,#6081,.T.);
#8089=ORIENTED_EDGE('',*,*,#6078,.T.);
#8090=ORIENTED_EDGE('',*,*,#6083,.T.);
#8091=ORIENTED_EDGE('',*,*,#6074,.T.);
#8092=ORIENTED_EDGE('',*,*,#6085,.T.);
#8093=ORIENTED_EDGE('',*,*,#6070,.T.);
#8094=ORIENTED_EDGE('',*,*,#6087,.T.);
#8095=ORIENTED_EDGE('',*,*,#6062,.T.);
#8096=ORIENTED_EDGE('',*,*,#6089,.T.);
#8097=ORIENTED_EDGE('',*,*,#6066,.T.);
#8098=ORIENTED_EDGE('',*,*,#6091,.T.);
#8099=ORIENTED_EDGE('',*,*,#6029,.T.);
#8100=ORIENTED_EDGE('',*,*,#6033,.T.);
#8101=ORIENTED_EDGE('',*,*,#6025,.T.);
#8102=ORIENTED_EDGE('',*,*,#6005,.T.);
#8103=ORIENTED_EDGE('',*,*,#6006,.T.);
#8104=ORIENTED_EDGE('',*,*,#6009,.T.);
#8105=ORIENTED_EDGE('',*,*,#6012,.T.);
#8106=ORIENTED_EDGE('',*,*,#6015,.T.);
#8107=ORIENTED_EDGE('',*,*,#6018,.T.);
#8108=ORIENTED_EDGE('',*,*,#6059,.T.);
#8109=ORIENTED_EDGE('',*,*,#6056,.T.);
#8110=ORIENTED_EDGE('',*,*,#6053,.T.);
#8111=ORIENTED_EDGE('',*,*,#6050,.T.);
#8112=ORIENTED_EDGE('',*,*,#6047,.T.);
#8113=ORIENTED_EDGE('',*,*,#6044,.F.);
#8114=ORIENTED_EDGE('',*,*,#6041,.T.);
#8115=ORIENTED_EDGE('',*,*,#6038,.F.);
#8116=ORIENTED_EDGE('',*,*,#5994,.T.);
#8117=ORIENTED_EDGE('',*,*,#6008,.F.);
#8118=ORIENTED_EDGE('',*,*,#5991,.T.);
#8119=ORIENTED_EDGE('',*,*,#6011,.F.);
#8120=ORIENTED_EDGE('',*,*,#6093,.F.);
#8121=ORIENTED_EDGE('',*,*,#6094,.T.);
#8122=ORIENTED_EDGE('',*,*,#6095,.F.);
#8123=ORIENTED_EDGE('',*,*,#6094,.F.);
#8124=ORIENTED_EDGE('',*,*,#6096,.F.);
#8125=ORIENTED_EDGE('',*,*,#6097,.F.);
#8126=ORIENTED_EDGE('',*,*,#6098,.T.);
#8127=ORIENTED_EDGE('',*,*,#6099,.F.);
#8128=ORIENTED_EDGE('',*,*,#6098,.F.);
#8129=ORIENTED_EDGE('',*,*,#6100,.F.);
#8130=ORIENTED_EDGE('',*,*,#6101,.T.);
#8131=ORIENTED_EDGE('',*,*,#6102,.F.);
#8132=ORIENTED_EDGE('',*,*,#6101,.F.);
#8133=ORIENTED_EDGE('',*,*,#6103,.F.);
#8134=ORIENTED_EDGE('',*,*,#6104,.F.);
#8135=ORIENTED_EDGE('',*,*,#6105,.T.);
#8136=ORIENTED_EDGE('',*,*,#6106,.F.);
#8137=ORIENTED_EDGE('',*,*,#6105,.F.);
#8138=ORIENTED_EDGE('',*,*,#6096,.T.);
#8139=ORIENTED_EDGE('',*,*,#6097,.T.);
#8140=ORIENTED_EDGE('',*,*,#6107,.T.);
#8141=ORIENTED_EDGE('',*,*,#6093,.T.);
#8142=ORIENTED_EDGE('',*,*,#6107,.F.);
#8143=ORIENTED_EDGE('',*,*,#6108,.F.);
#8144=ORIENTED_EDGE('',*,*,#6109,.T.);
#8145=ORIENTED_EDGE('',*,*,#6110,.T.);
#8146=ORIENTED_EDGE('',*,*,#6109,.F.);
#8147=ORIENTED_EDGE('',*,*,#6103,.T.);
#8148=ORIENTED_EDGE('',*,*,#6104,.T.);
#8149=ORIENTED_EDGE('',*,*,#6111,.T.);
#8150=ORIENTED_EDGE('',*,*,#6100,.T.);
#8151=ORIENTED_EDGE('',*,*,#6111,.F.);
#8152=ORIENTED_EDGE('',*,*,#6102,.T.);
#8153=ORIENTED_EDGE('',*,*,#6108,.T.);
#8154=ORIENTED_EDGE('',*,*,#6099,.T.);
#8155=ORIENTED_EDGE('',*,*,#6110,.F.);
#8156=ORIENTED_EDGE('',*,*,#6095,.T.);
#8157=ORIENTED_EDGE('',*,*,#6112,.T.);
#8158=ORIENTED_EDGE('',*,*,#6113,.T.);
#8159=ORIENTED_EDGE('',*,*,#6114,.T.);
#8160=ORIENTED_EDGE('',*,*,#6115,.F.);
#8161=ORIENTED_EDGE('',*,*,#6106,.T.);
#8162=ORIENTED_EDGE('',*,*,#6116,.F.);
#8163=ORIENTED_EDGE('',*,*,#6117,.F.);
#8164=ORIENTED_EDGE('',*,*,#6118,.F.);
#8165=ORIENTED_EDGE('',*,*,#6119,.T.);
#8166=ORIENTED_EDGE('',*,*,#6120,.T.);
#8167=ORIENTED_EDGE('',*,*,#6117,.T.);
#8168=ORIENTED_EDGE('',*,*,#6121,.F.);
#8169=ORIENTED_EDGE('',*,*,#6113,.F.);
#8170=ORIENTED_EDGE('',*,*,#6122,.T.);
#8171=ORIENTED_EDGE('',*,*,#6118,.T.);
#8172=ORIENTED_EDGE('',*,*,#6120,.F.);
#8173=ORIENTED_EDGE('',*,*,#6112,.F.);
#8174=ORIENTED_EDGE('',*,*,#6115,.T.);
#8175=ORIENTED_EDGE('',*,*,#6123,.T.);
#8176=ORIENTED_EDGE('',*,*,#6119,.F.);
#8177=ORIENTED_EDGE('',*,*,#6122,.F.);
#8178=ORIENTED_EDGE('',*,*,#6121,.T.);
#8179=ORIENTED_EDGE('',*,*,#6116,.T.);
#8180=ORIENTED_EDGE('',*,*,#6123,.F.);
#8181=ORIENTED_EDGE('',*,*,#6114,.F.);
#8182=ORIENTED_EDGE('',*,*,#6124,.F.);
#8183=ORIENTED_EDGE('',*,*,#6125,.T.);
#8184=ORIENTED_EDGE('',*,*,#6126,.T.);
#8185=ORIENTED_EDGE('',*,*,#6125,.F.);
#8186=ORIENTED_EDGE('',*,*,#6127,.F.);
#8187=ORIENTED_EDGE('',*,*,#6128,.T.);
#8188=ORIENTED_EDGE('',*,*,#6129,.F.);
#8189=ORIENTED_EDGE('',*,*,#6128,.F.);
#8190=ORIENTED_EDGE('',*,*,#6130,.F.);
#8191=ORIENTED_EDGE('',*,*,#6131,.F.);
#8192=ORIENTED_EDGE('',*,*,#6132,.T.);
#8193=ORIENTED_EDGE('',*,*,#6133,.F.);
#8194=ORIENTED_EDGE('',*,*,#6132,.F.);
#8195=ORIENTED_EDGE('',*,*,#6134,.F.);
#8196=ORIENTED_EDGE('',*,*,#6135,.T.);
#8197=ORIENTED_EDGE('',*,*,#6136,.F.);
#8198=ORIENTED_EDGE('',*,*,#6135,.F.);
#8199=ORIENTED_EDGE('',*,*,#6137,.F.);
#8200=ORIENTED_EDGE('',*,*,#6138,.F.);
#8201=ORIENTED_EDGE('',*,*,#6139,.T.);
#8202=ORIENTED_EDGE('',*,*,#6140,.F.);
#8203=ORIENTED_EDGE('',*,*,#6139,.F.);
#8204=ORIENTED_EDGE('',*,*,#6130,.T.);
#8205=ORIENTED_EDGE('',*,*,#6131,.T.);
#8206=ORIENTED_EDGE('',*,*,#6141,.T.);
#8207=ORIENTED_EDGE('',*,*,#6127,.T.);
#8208=ORIENTED_EDGE('',*,*,#6141,.F.);
#8209=ORIENTED_EDGE('',*,*,#6142,.F.);
#8210=ORIENTED_EDGE('',*,*,#6143,.T.);
#8211=ORIENTED_EDGE('',*,*,#6144,.T.);
#8212=ORIENTED_EDGE('',*,*,#6143,.F.);
#8213=ORIENTED_EDGE('',*,*,#6137,.T.);
#8214=ORIENTED_EDGE('',*,*,#6138,.T.);
#8215=ORIENTED_EDGE('',*,*,#6145,.T.);
#8216=ORIENTED_EDGE('',*,*,#6134,.T.);
#8217=ORIENTED_EDGE('',*,*,#6145,.F.);
#8218=ORIENTED_EDGE('',*,*,#6129,.T.);
#8219=ORIENTED_EDGE('',*,*,#6124,.T.);
#8220=ORIENTED_EDGE('',*,*,#6140,.T.);
#8221=ORIENTED_EDGE('',*,*,#6126,.F.);
#8222=ORIENTED_EDGE('',*,*,#6136,.T.);
#8223=ORIENTED_EDGE('',*,*,#6142,.T.);
#8224=ORIENTED_EDGE('',*,*,#6133,.T.);
#8225=ORIENTED_EDGE('',*,*,#6144,.F.);
#8226=ORIENTED_EDGE('',*,*,#6146,.F.);
#8227=ORIENTED_EDGE('',*,*,#6147,.T.);
#8228=ORIENTED_EDGE('',*,*,#6148,.F.);
#8229=ORIENTED_EDGE('',*,*,#6149,.F.);
#8230=ORIENTED_EDGE('',*,*,#6147,.F.);
#8231=ORIENTED_EDGE('',*,*,#6150,.T.);
#8232=ORIENTED_EDGE('',*,*,#6151,.T.);
#8233=ORIENTED_EDGE('',*,*,#6148,.T.);
#8234=ORIENTED_EDGE('',*,*,#6149,.T.);
#8235=ORIENTED_EDGE('',*,*,#6151,.F.);
#8236=ORIENTED_EDGE('',*,*,#6152,.F.);
#8237=ORIENTED_EDGE('',*,*,#6153,.T.);
#8238=ORIENTED_EDGE('',*,*,#6154,.T.);
#8239=ORIENTED_EDGE('',*,*,#6153,.F.);
#8240=ORIENTED_EDGE('',*,*,#6155,.F.);
#8241=ORIENTED_EDGE('',*,*,#6156,.T.);
#8242=ORIENTED_EDGE('',*,*,#6157,.T.);
#8243=ORIENTED_EDGE('',*,*,#6156,.F.);
#8244=ORIENTED_EDGE('',*,*,#6158,.F.);
#8245=ORIENTED_EDGE('',*,*,#6159,.T.);
#8246=ORIENTED_EDGE('',*,*,#6160,.T.);
#8247=ORIENTED_EDGE('',*,*,#6159,.F.);
#8248=ORIENTED_EDGE('',*,*,#6161,.F.);
#8249=ORIENTED_EDGE('',*,*,#6162,.T.);
#8250=ORIENTED_EDGE('',*,*,#6163,.T.);
#8251=ORIENTED_EDGE('',*,*,#6162,.F.);
#8252=ORIENTED_EDGE('',*,*,#6164,.T.);
#8253=ORIENTED_EDGE('',*,*,#6165,.T.);
#8254=ORIENTED_EDGE('',*,*,#6166,.T.);
#8255=ORIENTED_EDGE('',*,*,#6165,.F.);
#8256=ORIENTED_EDGE('',*,*,#6167,.T.);
#8257=ORIENTED_EDGE('',*,*,#6168,.T.);
#8258=ORIENTED_EDGE('',*,*,#6169,.F.);
#8259=ORIENTED_EDGE('',*,*,#6170,.T.);
#8260=ORIENTED_EDGE('',*,*,#6171,.F.);
#8261=ORIENTED_EDGE('',*,*,#6172,.T.);
#8262=ORIENTED_EDGE('',*,*,#6173,.F.);
#8263=ORIENTED_EDGE('',*,*,#6174,.T.);
#8264=ORIENTED_EDGE('',*,*,#6175,.F.);
#8265=ORIENTED_EDGE('',*,*,#6176,.T.);
#8266=ORIENTED_EDGE('',*,*,#6177,.F.);
#8267=ORIENTED_EDGE('',*,*,#6168,.F.);
#8268=ORIENTED_EDGE('',*,*,#6178,.F.);
#8269=ORIENTED_EDGE('',*,*,#6179,.T.);
#8270=ORIENTED_EDGE('',*,*,#6180,.F.);
#8271=ORIENTED_EDGE('',*,*,#6181,.F.);
#8272=ORIENTED_EDGE('',*,*,#6182,.T.);
#8273=ORIENTED_EDGE('',*,*,#6183,.T.);
#8274=ORIENTED_EDGE('',*,*,#6184,.T.);
#8275=ORIENTED_EDGE('',*,*,#6185,.F.);
#8276=ORIENTED_EDGE('',*,*,#6186,.F.);
#8277=ORIENTED_EDGE('',*,*,#6187,.T.);
#8278=ORIENTED_EDGE('',*,*,#6188,.T.);
#8279=ORIENTED_EDGE('',*,*,#6189,.T.);
#8280=ORIENTED_EDGE('',*,*,#6190,.T.);
#8281=ORIENTED_EDGE('',*,*,#6191,.T.);
#8282=ORIENTED_EDGE('',*,*,#6192,.T.);
#8283=ORIENTED_EDGE('',*,*,#6193,.T.);
#8284=ORIENTED_EDGE('',*,*,#6194,.T.);
#8285=ORIENTED_EDGE('',*,*,#6195,.T.);
#8286=ORIENTED_EDGE('',*,*,#6196,.T.);
#8287=ORIENTED_EDGE('',*,*,#6197,.T.);
#8288=ORIENTED_EDGE('',*,*,#6198,.T.);
#8289=ORIENTED_EDGE('',*,*,#6199,.T.);
#8290=ORIENTED_EDGE('',*,*,#6200,.T.);
#8291=ORIENTED_EDGE('',*,*,#6201,.T.);
#8292=ORIENTED_EDGE('',*,*,#6192,.F.);
#8293=ORIENTED_EDGE('',*,*,#6202,.F.);
#8294=ORIENTED_EDGE('',*,*,#6203,.F.);
#8295=ORIENTED_EDGE('',*,*,#6204,.F.);
#8296=ORIENTED_EDGE('',*,*,#6205,.F.);
#8297=ORIENTED_EDGE('',*,*,#6206,.F.);
#8298=ORIENTED_EDGE('',*,*,#6207,.F.);
#8299=ORIENTED_EDGE('',*,*,#6208,.F.);
#8300=ORIENTED_EDGE('',*,*,#6209,.F.);
#8301=ORIENTED_EDGE('',*,*,#6210,.T.);
#8302=ORIENTED_EDGE('',*,*,#6190,.F.);
#8303=ORIENTED_EDGE('',*,*,#6167,.F.);
#8304=ORIENTED_EDGE('',*,*,#6163,.F.);
#8305=ORIENTED_EDGE('',*,*,#6160,.F.);
#8306=ORIENTED_EDGE('',*,*,#6157,.F.);
#8307=ORIENTED_EDGE('',*,*,#6154,.F.);
#8308=ORIENTED_EDGE('',*,*,#6150,.F.);
#8309=ORIENTED_EDGE('',*,*,#6211,.F.);
#8310=ORIENTED_EDGE('',*,*,#6212,.F.);
#8311=ORIENTED_EDGE('',*,*,#6205,.T.);
#8312=ORIENTED_EDGE('',*,*,#6213,.T.);
#8313=ORIENTED_EDGE('',*,*,#6214,.F.);
#8314=ORIENTED_EDGE('',*,*,#6215,.F.);
#8315=ORIENTED_EDGE('',*,*,#6216,.F.);
#8316=ORIENTED_EDGE('',*,*,#6217,.F.);
#8317=ORIENTED_EDGE('',*,*,#6197,.F.);
#8318=ORIENTED_EDGE('',*,*,#6218,.T.);
#8319=ORIENTED_EDGE('',*,*,#6193,.F.);
#8320=ORIENTED_EDGE('',*,*,#6201,.F.);
#8321=ORIENTED_EDGE('',*,*,#6219,.T.);
#8322=ORIENTED_EDGE('',*,*,#6210,.F.);
#8323=ORIENTED_EDGE('',*,*,#6220,.T.);
#8324=ORIENTED_EDGE('',*,*,#6221,.F.);
#8325=ORIENTED_EDGE('',*,*,#6186,.T.);
#8326=ORIENTED_EDGE('',*,*,#6184,.F.);
#8327=ORIENTED_EDGE('',*,*,#6222,.F.);
#8328=ORIENTED_EDGE('',*,*,#6223,.F.);
#8329=ORIENTED_EDGE('',*,*,#6224,.F.);
#8330=ORIENTED_EDGE('',*,*,#6220,.F.);
#8331=ORIENTED_EDGE('',*,*,#6209,.T.);
#8332=ORIENTED_EDGE('',*,*,#6225,.T.);
#8333=ORIENTED_EDGE('',*,*,#6226,.T.);
#8334=ORIENTED_EDGE('',*,*,#6227,.T.);
#8335=ORIENTED_EDGE('',*,*,#6189,.F.);
#8336=ORIENTED_EDGE('',*,*,#6228,.F.);
#8337=ORIENTED_EDGE('',*,*,#6202,.T.);
#8338=ORIENTED_EDGE('',*,*,#6229,.T.);
#8339=ORIENTED_EDGE('',*,*,#6230,.F.);
#8340=ORIENTED_EDGE('',*,*,#6231,.F.);
#8341=ORIENTED_EDGE('',*,*,#6188,.F.);
#8342=ORIENTED_EDGE('',*,*,#6232,.T.);
#8343=ORIENTED_EDGE('',*,*,#6226,.F.);
#8344=ORIENTED_EDGE('',*,*,#6225,.F.);
#8345=ORIENTED_EDGE('',*,*,#6208,.T.);
#8346=ORIENTED_EDGE('',*,*,#6233,.T.);
#8347=ORIENTED_EDGE('',*,*,#6234,.F.);
#8348=ORIENTED_EDGE('',*,*,#6235,.F.);
#8349=ORIENTED_EDGE('',*,*,#6203,.T.);
#8350=ORIENTED_EDGE('',*,*,#6228,.T.);
#8351=ORIENTED_EDGE('',*,*,#6231,.T.);
#8352=ORIENTED_EDGE('',*,*,#6236,.F.);
#8353=ORIENTED_EDGE('',*,*,#6213,.F.);
#8354=ORIENTED_EDGE('',*,*,#6204,.T.);
#8355=ORIENTED_EDGE('',*,*,#6235,.T.);
#8356=ORIENTED_EDGE('',*,*,#6237,.F.);
#8357=ORIENTED_EDGE('',*,*,#6238,.F.);
#8358=ORIENTED_EDGE('',*,*,#6206,.T.);
#8359=ORIENTED_EDGE('',*,*,#6212,.T.);
#8360=ORIENTED_EDGE('',*,*,#6239,.F.);
#8361=ORIENTED_EDGE('',*,*,#6229,.F.);
#8362=ORIENTED_EDGE('',*,*,#6233,.F.);
#8363=ORIENTED_EDGE('',*,*,#6207,.T.);
#8364=ORIENTED_EDGE('',*,*,#6238,.T.);
#8365=ORIENTED_EDGE('',*,*,#6230,.T.);
#8366=ORIENTED_EDGE('',*,*,#6239,.T.);
#8367=ORIENTED_EDGE('',*,*,#6237,.T.);
#8368=ORIENTED_EDGE('',*,*,#6211,.T.);
#8369=ORIENTED_EDGE('',*,*,#6236,.T.);
#8370=ORIENTED_EDGE('',*,*,#6234,.T.);
#8371=ORIENTED_EDGE('',*,*,#6152,.T.);
#8372=ORIENTED_EDGE('',*,*,#6155,.T.);
#8373=ORIENTED_EDGE('',*,*,#6158,.T.);
#8374=ORIENTED_EDGE('',*,*,#6161,.T.);
#8375=ORIENTED_EDGE('',*,*,#6191,.F.);
#8376=ORIENTED_EDGE('',*,*,#6221,.T.);
#8377=ORIENTED_EDGE('',*,*,#6227,.F.);
#8378=ORIENTED_EDGE('',*,*,#6232,.F.);
#8379=ORIENTED_EDGE('',*,*,#6187,.F.);
#8380=ORIENTED_EDGE('',*,*,#6240,.F.);
#8381=ORIENTED_EDGE('',*,*,#6178,.T.);
#8382=ORIENTED_EDGE('',*,*,#6241,.T.);
#8383=ORIENTED_EDGE('',*,*,#6223,.T.);
#8384=ORIENTED_EDGE('',*,*,#6183,.F.);
#8385=ORIENTED_EDGE('',*,*,#6242,.T.);
#8386=ORIENTED_EDGE('',*,*,#6240,.T.);
#8387=ORIENTED_EDGE('',*,*,#6222,.T.);
#8388=ORIENTED_EDGE('',*,*,#6241,.F.);
#8389=ORIENTED_EDGE('',*,*,#6243,.T.);
#8390=ORIENTED_EDGE('',*,*,#6185,.T.);
#8391=ORIENTED_EDGE('',*,*,#6224,.T.);
#8392=ORIENTED_EDGE('',*,*,#6244,.T.);
#8393=ORIENTED_EDGE('',*,*,#6245,.T.);
#8394=ORIENTED_EDGE('',*,*,#6180,.T.);
#8395=ORIENTED_EDGE('',*,*,#6246,.T.);
#8396=ORIENTED_EDGE('',*,*,#6179,.F.);
#8397=ORIENTED_EDGE('',*,*,#6242,.F.);
#8398=ORIENTED_EDGE('',*,*,#6247,.F.);
#8399=ORIENTED_EDGE('',*,*,#6246,.F.);
#8400=ORIENTED_EDGE('',*,*,#6247,.T.);
#8401=ORIENTED_EDGE('',*,*,#6182,.F.);
#8402=ORIENTED_EDGE('',*,*,#6248,.F.);
#8403=ORIENTED_EDGE('',*,*,#6244,.F.);
#8404=ORIENTED_EDGE('',*,*,#6248,.T.);
#8405=ORIENTED_EDGE('',*,*,#6243,.F.);
#8406=ORIENTED_EDGE('',*,*,#6181,.T.);
#8407=ORIENTED_EDGE('',*,*,#6245,.F.);
#8408=ORIENTED_EDGE('',*,*,#6249,.F.);
#8409=ORIENTED_EDGE('',*,*,#6169,.T.);
#8410=ORIENTED_EDGE('',*,*,#6177,.T.);
#8411=ORIENTED_EDGE('',*,*,#6250,.F.);
#8412=ORIENTED_EDGE('',*,*,#6173,.T.);
#8413=ORIENTED_EDGE('',*,*,#6175,.T.);
#8414=ORIENTED_EDGE('',*,*,#6251,.T.);
#8415=ORIENTED_EDGE('',*,*,#6250,.T.);
#8416=ORIENTED_EDGE('',*,*,#6176,.F.);
#8417=ORIENTED_EDGE('',*,*,#6251,.F.);
#8418=ORIENTED_EDGE('',*,*,#6174,.F.);
#8419=ORIENTED_EDGE('',*,*,#6171,.T.);
#8420=ORIENTED_EDGE('',*,*,#6252,.T.);
#8421=ORIENTED_EDGE('',*,*,#6249,.T.);
#8422=ORIENTED_EDGE('',*,*,#6172,.F.);
#8423=ORIENTED_EDGE('',*,*,#6252,.F.);
#8424=ORIENTED_EDGE('',*,*,#6170,.F.);
#8425=ORIENTED_EDGE('',*,*,#6253,.T.);
#8426=ORIENTED_EDGE('',*,*,#6198,.F.);
#8427=ORIENTED_EDGE('',*,*,#6219,.F.);
#8428=ORIENTED_EDGE('',*,*,#6200,.F.);
#8429=ORIENTED_EDGE('',*,*,#6253,.F.);
#8430=ORIENTED_EDGE('',*,*,#6199,.F.);
#8431=ORIENTED_EDGE('',*,*,#6254,.T.);
#8432=ORIENTED_EDGE('',*,*,#6194,.F.);
#8433=ORIENTED_EDGE('',*,*,#6218,.F.);
#8434=ORIENTED_EDGE('',*,*,#6196,.F.);
#8435=ORIENTED_EDGE('',*,*,#6254,.F.);
#8436=ORIENTED_EDGE('',*,*,#6195,.F.);
#8437=ORIENTED_EDGE('',*,*,#6215,.T.);
#8438=ORIENTED_EDGE('',*,*,#6255,.F.);
#8439=ORIENTED_EDGE('',*,*,#6256,.F.);
#8440=ORIENTED_EDGE('',*,*,#6257,.T.);
#8441=ORIENTED_EDGE('',*,*,#6164,.F.);
#8442=ORIENTED_EDGE('',*,*,#6214,.T.);
#8443=ORIENTED_EDGE('',*,*,#6258,.F.);
#8444=ORIENTED_EDGE('',*,*,#6259,.F.);
#8445=ORIENTED_EDGE('',*,*,#6255,.T.);
#8446=ORIENTED_EDGE('',*,*,#6217,.T.);
#8447=ORIENTED_EDGE('',*,*,#6260,.F.);
#8448=ORIENTED_EDGE('',*,*,#6261,.F.);
#8449=ORIENTED_EDGE('',*,*,#6258,.T.);
#8450=ORIENTED_EDGE('',*,*,#6166,.F.);
#8451=ORIENTED_EDGE('',*,*,#6216,.T.);
#8452=ORIENTED_EDGE('',*,*,#6257,.F.);
#8453=ORIENTED_EDGE('',*,*,#6262,.F.);
#8454=ORIENTED_EDGE('',*,*,#6260,.T.);
#8455=ORIENTED_EDGE('',*,*,#6256,.T.);
#8456=ORIENTED_EDGE('',*,*,#6259,.T.);
#8457=ORIENTED_EDGE('',*,*,#6261,.T.);
#8458=ORIENTED_EDGE('',*,*,#6262,.T.);
#8459=ORIENTED_EDGE('',*,*,#6146,.T.);
#8460=ORIENTED_EDGE('',*,*,#6263,.T.);
#8461=ORIENTED_EDGE('',*,*,#6264,.T.);
#8462=ORIENTED_EDGE('',*,*,#6265,.F.);
#8463=ORIENTED_EDGE('',*,*,#6266,.F.);
#8464=ORIENTED_EDGE('',*,*,#6267,.F.);
#8465=ORIENTED_EDGE('',*,*,#6268,.T.);
#8466=ORIENTED_EDGE('',*,*,#6269,.T.);
#8467=ORIENTED_EDGE('',*,*,#6270,.F.);
#8468=ORIENTED_EDGE('',*,*,#6267,.T.);
#8469=ORIENTED_EDGE('',*,*,#6271,.T.);
#8470=ORIENTED_EDGE('',*,*,#6272,.T.);
#8471=ORIENTED_EDGE('',*,*,#6273,.T.);
#8472=ORIENTED_EDGE('',*,*,#6274,.F.);
#8473=ORIENTED_EDGE('',*,*,#6263,.F.);
#8474=ORIENTED_EDGE('',*,*,#6275,.F.);
#8475=ORIENTED_EDGE('',*,*,#6276,.F.);
#8476=ORIENTED_EDGE('',*,*,#6269,.F.);
#8477=ORIENTED_EDGE('',*,*,#6277,.F.);
#8478=ORIENTED_EDGE('',*,*,#6278,.F.);
#8479=ORIENTED_EDGE('',*,*,#6279,.F.);
#8480=ORIENTED_EDGE('',*,*,#6265,.T.);
#8481=ORIENTED_EDGE('',*,*,#6280,.T.);
#8482=ORIENTED_EDGE('',*,*,#6281,.T.);
#8483=ORIENTED_EDGE('',*,*,#6282,.T.);
#8484=ORIENTED_EDGE('',*,*,#6279,.T.);
#8485=ORIENTED_EDGE('',*,*,#6283,.F.);
#8486=ORIENTED_EDGE('',*,*,#6271,.F.);
#8487=ORIENTED_EDGE('',*,*,#6270,.T.);
#8488=ORIENTED_EDGE('',*,*,#6278,.T.);
#8489=ORIENTED_EDGE('',*,*,#6284,.F.);
#8490=ORIENTED_EDGE('',*,*,#6272,.F.);
#8491=ORIENTED_EDGE('',*,*,#6283,.T.);
#8492=ORIENTED_EDGE('',*,*,#6277,.T.);
#8493=ORIENTED_EDGE('',*,*,#6268,.F.);
#8494=ORIENTED_EDGE('',*,*,#6273,.F.);
#8495=ORIENTED_EDGE('',*,*,#6284,.T.);
#8496=ORIENTED_EDGE('',*,*,#6280,.F.);
#8497=ORIENTED_EDGE('',*,*,#6264,.F.);
#8498=ORIENTED_EDGE('',*,*,#6274,.T.);
#8499=ORIENTED_EDGE('',*,*,#6285,.T.);
#8500=ORIENTED_EDGE('',*,*,#6281,.F.);
#8501=ORIENTED_EDGE('',*,*,#6285,.F.);
#8502=ORIENTED_EDGE('',*,*,#6276,.T.);
#8503=ORIENTED_EDGE('',*,*,#6286,.T.);
#8504=ORIENTED_EDGE('',*,*,#6282,.F.);
#8505=ORIENTED_EDGE('',*,*,#6286,.F.);
#8506=ORIENTED_EDGE('',*,*,#6275,.T.);
#8507=ORIENTED_EDGE('',*,*,#6266,.T.);
#8508=ORIENTED_EDGE('',*,*,#6287,.T.);
#8509=ORIENTED_EDGE('',*,*,#6288,.T.);
#8510=ORIENTED_EDGE('',*,*,#6289,.F.);
#8511=ORIENTED_EDGE('',*,*,#6290,.F.);
#8512=ORIENTED_EDGE('',*,*,#6291,.F.);
#8513=ORIENTED_EDGE('',*,*,#6292,.T.);
#8514=ORIENTED_EDGE('',*,*,#6293,.T.);
#8515=ORIENTED_EDGE('',*,*,#6294,.F.);
#8516=ORIENTED_EDGE('',*,*,#6291,.T.);
#8517=ORIENTED_EDGE('',*,*,#6295,.T.);
#8518=ORIENTED_EDGE('',*,*,#6296,.T.);
#8519=ORIENTED_EDGE('',*,*,#6297,.T.);
#8520=ORIENTED_EDGE('',*,*,#6298,.T.);
#8521=ORIENTED_EDGE('',*,*,#6299,.T.);
#8522=ORIENTED_EDGE('',*,*,#6300,.F.);
#8523=ORIENTED_EDGE('',*,*,#6287,.F.);
#8524=ORIENTED_EDGE('',*,*,#6301,.F.);
#8525=ORIENTED_EDGE('',*,*,#6302,.F.);
#8526=ORIENTED_EDGE('',*,*,#6303,.F.);
#8527=ORIENTED_EDGE('',*,*,#6304,.F.);
#8528=ORIENTED_EDGE('',*,*,#6293,.F.);
#8529=ORIENTED_EDGE('',*,*,#6305,.F.);
#8530=ORIENTED_EDGE('',*,*,#6306,.F.);
#8531=ORIENTED_EDGE('',*,*,#6307,.F.);
#8532=ORIENTED_EDGE('',*,*,#6308,.F.);
#8533=ORIENTED_EDGE('',*,*,#6309,.F.);
#8534=ORIENTED_EDGE('',*,*,#6289,.T.);
#8535=ORIENTED_EDGE('',*,*,#6310,.T.);
#8536=ORIENTED_EDGE('',*,*,#6311,.T.);
#8537=ORIENTED_EDGE('',*,*,#6312,.T.);
#8538=ORIENTED_EDGE('',*,*,#6313,.T.);
#8539=ORIENTED_EDGE('',*,*,#6314,.T.);
#8540=ORIENTED_EDGE('',*,*,#6309,.T.);
#8541=ORIENTED_EDGE('',*,*,#6315,.F.);
#8542=ORIENTED_EDGE('',*,*,#6295,.F.);
#8543=ORIENTED_EDGE('',*,*,#6294,.T.);
#8544=ORIENTED_EDGE('',*,*,#6308,.T.);
#8545=ORIENTED_EDGE('',*,*,#6316,.F.);
#8546=ORIENTED_EDGE('',*,*,#6296,.F.);
#8547=ORIENTED_EDGE('',*,*,#6315,.T.);
#8548=ORIENTED_EDGE('',*,*,#6307,.T.);
#8549=ORIENTED_EDGE('',*,*,#6317,.F.);
#8550=ORIENTED_EDGE('',*,*,#6297,.F.);
#8551=ORIENTED_EDGE('',*,*,#6316,.T.);
#8552=ORIENTED_EDGE('',*,*,#6306,.T.);
#8553=ORIENTED_EDGE('',*,*,#6318,.F.);
#8554=ORIENTED_EDGE('',*,*,#6298,.F.);
#8555=ORIENTED_EDGE('',*,*,#6317,.T.);
#8556=ORIENTED_EDGE('',*,*,#6305,.T.);
#8557=ORIENTED_EDGE('',*,*,#6292,.F.);
#8558=ORIENTED_EDGE('',*,*,#6299,.F.);
#8559=ORIENTED_EDGE('',*,*,#6318,.T.);
#8560=ORIENTED_EDGE('',*,*,#6310,.F.);
#8561=ORIENTED_EDGE('',*,*,#6288,.F.);
#8562=ORIENTED_EDGE('',*,*,#6300,.T.);
#8563=ORIENTED_EDGE('',*,*,#6319,.T.);
#8564=ORIENTED_EDGE('',*,*,#6311,.F.);
#8565=ORIENTED_EDGE('',*,*,#6319,.F.);
#8566=ORIENTED_EDGE('',*,*,#6304,.T.);
#8567=ORIENTED_EDGE('',*,*,#6320,.T.);
#8568=ORIENTED_EDGE('',*,*,#6312,.F.);
#8569=ORIENTED_EDGE('',*,*,#6320,.F.);
#8570=ORIENTED_EDGE('',*,*,#6303,.T.);
#8571=ORIENTED_EDGE('',*,*,#6321,.T.);
#8572=ORIENTED_EDGE('',*,*,#6313,.F.);
#8573=ORIENTED_EDGE('',*,*,#6321,.F.);
#8574=ORIENTED_EDGE('',*,*,#6302,.T.);
#8575=ORIENTED_EDGE('',*,*,#6322,.T.);
#8576=ORIENTED_EDGE('',*,*,#6314,.F.);
#8577=ORIENTED_EDGE('',*,*,#6322,.F.);
#8578=ORIENTED_EDGE('',*,*,#6301,.T.);
#8579=ORIENTED_EDGE('',*,*,#6290,.T.);
#8580=ORIENTED_EDGE('',*,*,#6323,.T.);
#8581=ORIENTED_EDGE('',*,*,#6324,.T.);
#8582=ORIENTED_EDGE('',*,*,#6325,.F.);
#8583=ORIENTED_EDGE('',*,*,#6326,.F.);
#8584=ORIENTED_EDGE('',*,*,#6327,.T.);
#8585=ORIENTED_EDGE('',*,*,#6328,.T.);
#8586=ORIENTED_EDGE('',*,*,#6329,.T.);
#8587=ORIENTED_EDGE('',*,*,#6330,.T.);
#8588=ORIENTED_EDGE('',*,*,#6331,.T.);
#8589=ORIENTED_EDGE('',*,*,#6332,.T.);
#8590=ORIENTED_EDGE('',*,*,#6333,.T.);
#8591=ORIENTED_EDGE('',*,*,#6334,.T.);
#8592=ORIENTED_EDGE('',*,*,#6335,.T.);
#8593=ORIENTED_EDGE('',*,*,#6336,.T.);
#8594=ORIENTED_EDGE('',*,*,#6337,.T.);
#8595=ORIENTED_EDGE('',*,*,#6338,.T.);
#8596=ORIENTED_EDGE('',*,*,#6339,.T.);
#8597=ORIENTED_EDGE('',*,*,#6340,.T.);
#8598=ORIENTED_EDGE('',*,*,#6341,.T.);
#8599=ORIENTED_EDGE('',*,*,#6342,.T.);
#8600=ORIENTED_EDGE('',*,*,#6343,.T.);
#8601=ORIENTED_EDGE('',*,*,#6344,.T.);
#8602=ORIENTED_EDGE('',*,*,#6345,.T.);
#8603=ORIENTED_EDGE('',*,*,#6346,.T.);
#8604=ORIENTED_EDGE('',*,*,#6347,.T.);
#8605=ORIENTED_EDGE('',*,*,#6348,.T.);
#8606=ORIENTED_EDGE('',*,*,#6349,.T.);
#8607=ORIENTED_EDGE('',*,*,#6350,.T.);
#8608=ORIENTED_EDGE('',*,*,#6351,.T.);
#8609=ORIENTED_EDGE('',*,*,#6352,.T.);
#8610=ORIENTED_EDGE('',*,*,#6353,.T.);
#8611=ORIENTED_EDGE('',*,*,#6354,.T.);
#8612=ORIENTED_EDGE('',*,*,#6355,.T.);
#8613=ORIENTED_EDGE('',*,*,#6356,.T.);
#8614=ORIENTED_EDGE('',*,*,#6357,.T.);
#8615=ORIENTED_EDGE('',*,*,#6358,.T.);
#8616=ORIENTED_EDGE('',*,*,#6359,.T.);
#8617=ORIENTED_EDGE('',*,*,#6360,.T.);
#8618=ORIENTED_EDGE('',*,*,#6361,.T.);
#8619=ORIENTED_EDGE('',*,*,#6362,.T.);
#8620=ORIENTED_EDGE('',*,*,#6363,.T.);
#8621=ORIENTED_EDGE('',*,*,#6364,.T.);
#8622=ORIENTED_EDGE('',*,*,#6365,.T.);
#8623=ORIENTED_EDGE('',*,*,#6366,.T.);
#8624=ORIENTED_EDGE('',*,*,#6367,.T.);
#8625=ORIENTED_EDGE('',*,*,#6368,.T.);
#8626=ORIENTED_EDGE('',*,*,#6369,.T.);
#8627=ORIENTED_EDGE('',*,*,#6370,.T.);
#8628=ORIENTED_EDGE('',*,*,#6371,.T.);
#8629=ORIENTED_EDGE('',*,*,#6372,.T.);
#8630=ORIENTED_EDGE('',*,*,#6373,.T.);
#8631=ORIENTED_EDGE('',*,*,#6374,.T.);
#8632=ORIENTED_EDGE('',*,*,#6375,.T.);
#8633=ORIENTED_EDGE('',*,*,#6376,.T.);
#8634=ORIENTED_EDGE('',*,*,#6377,.T.);
#8635=ORIENTED_EDGE('',*,*,#6378,.T.);
#8636=ORIENTED_EDGE('',*,*,#6379,.T.);
#8637=ORIENTED_EDGE('',*,*,#6380,.T.);
#8638=ORIENTED_EDGE('',*,*,#6381,.T.);
#8639=ORIENTED_EDGE('',*,*,#6382,.T.);
#8640=ORIENTED_EDGE('',*,*,#6383,.T.);
#8641=ORIENTED_EDGE('',*,*,#6384,.T.);
#8642=ORIENTED_EDGE('',*,*,#6385,.T.);
#8643=ORIENTED_EDGE('',*,*,#6386,.T.);
#8644=ORIENTED_EDGE('',*,*,#6387,.T.);
#8645=ORIENTED_EDGE('',*,*,#6388,.T.);
#8646=ORIENTED_EDGE('',*,*,#6389,.T.);
#8647=ORIENTED_EDGE('',*,*,#6390,.T.);
#8648=ORIENTED_EDGE('',*,*,#6391,.T.);
#8649=ORIENTED_EDGE('',*,*,#6392,.T.);
#8650=ORIENTED_EDGE('',*,*,#6393,.T.);
#8651=ORIENTED_EDGE('',*,*,#6394,.T.);
#8652=ORIENTED_EDGE('',*,*,#6395,.T.);
#8653=ORIENTED_EDGE('',*,*,#6396,.T.);
#8654=ORIENTED_EDGE('',*,*,#6397,.T.);
#8655=ORIENTED_EDGE('',*,*,#6398,.T.);
#8656=ORIENTED_EDGE('',*,*,#6399,.T.);
#8657=ORIENTED_EDGE('',*,*,#6400,.T.);
#8658=ORIENTED_EDGE('',*,*,#6401,.T.);
#8659=ORIENTED_EDGE('',*,*,#6402,.T.);
#8660=ORIENTED_EDGE('',*,*,#6403,.T.);
#8661=ORIENTED_EDGE('',*,*,#6404,.T.);
#8662=ORIENTED_EDGE('',*,*,#6405,.T.);
#8663=ORIENTED_EDGE('',*,*,#6406,.T.);
#8664=ORIENTED_EDGE('',*,*,#6407,.T.);
#8665=ORIENTED_EDGE('',*,*,#6408,.T.);
#8666=ORIENTED_EDGE('',*,*,#6409,.T.);
#8667=ORIENTED_EDGE('',*,*,#6410,.T.);
#8668=ORIENTED_EDGE('',*,*,#6411,.T.);
#8669=ORIENTED_EDGE('',*,*,#6412,.T.);
#8670=ORIENTED_EDGE('',*,*,#6413,.T.);
#8671=ORIENTED_EDGE('',*,*,#6414,.T.);
#8672=ORIENTED_EDGE('',*,*,#6415,.T.);
#8673=ORIENTED_EDGE('',*,*,#6416,.T.);
#8674=ORIENTED_EDGE('',*,*,#6417,.T.);
#8675=ORIENTED_EDGE('',*,*,#6418,.T.);
#8676=ORIENTED_EDGE('',*,*,#6419,.T.);
#8677=ORIENTED_EDGE('',*,*,#6420,.T.);
#8678=ORIENTED_EDGE('',*,*,#6421,.T.);
#8679=ORIENTED_EDGE('',*,*,#6422,.T.);
#8680=ORIENTED_EDGE('',*,*,#6423,.T.);
#8681=ORIENTED_EDGE('',*,*,#6424,.T.);
#8682=ORIENTED_EDGE('',*,*,#6425,.T.);
#8683=ORIENTED_EDGE('',*,*,#6426,.T.);
#8684=ORIENTED_EDGE('',*,*,#6427,.T.);
#8685=ORIENTED_EDGE('',*,*,#6428,.T.);
#8686=ORIENTED_EDGE('',*,*,#6429,.T.);
#8687=ORIENTED_EDGE('',*,*,#6430,.T.);
#8688=ORIENTED_EDGE('',*,*,#6431,.T.);
#8689=ORIENTED_EDGE('',*,*,#6432,.T.);
#8690=ORIENTED_EDGE('',*,*,#6433,.T.);
#8691=ORIENTED_EDGE('',*,*,#6434,.T.);
#8692=ORIENTED_EDGE('',*,*,#6435,.T.);
#8693=ORIENTED_EDGE('',*,*,#6436,.T.);
#8694=ORIENTED_EDGE('',*,*,#6437,.T.);
#8695=ORIENTED_EDGE('',*,*,#6438,.T.);
#8696=ORIENTED_EDGE('',*,*,#6439,.T.);
#8697=ORIENTED_EDGE('',*,*,#6440,.T.);
#8698=ORIENTED_EDGE('',*,*,#6441,.T.);
#8699=ORIENTED_EDGE('',*,*,#6442,.T.);
#8700=ORIENTED_EDGE('',*,*,#6443,.F.);
#8701=ORIENTED_EDGE('',*,*,#6444,.F.);
#8702=ORIENTED_EDGE('',*,*,#6445,.F.);
#8703=ORIENTED_EDGE('',*,*,#6446,.F.);
#8704=ORIENTED_EDGE('',*,*,#6447,.F.);
#8705=ORIENTED_EDGE('',*,*,#6448,.F.);
#8706=ORIENTED_EDGE('',*,*,#6449,.F.);
#8707=ORIENTED_EDGE('',*,*,#6450,.F.);
#8708=ORIENTED_EDGE('',*,*,#6451,.F.);
#8709=ORIENTED_EDGE('',*,*,#6452,.F.);
#8710=ORIENTED_EDGE('',*,*,#6453,.F.);
#8711=ORIENTED_EDGE('',*,*,#6454,.F.);
#8712=ORIENTED_EDGE('',*,*,#6455,.F.);
#8713=ORIENTED_EDGE('',*,*,#6456,.F.);
#8714=ORIENTED_EDGE('',*,*,#6457,.F.);
#8715=ORIENTED_EDGE('',*,*,#6458,.F.);
#8716=ORIENTED_EDGE('',*,*,#6459,.F.);
#8717=ORIENTED_EDGE('',*,*,#6460,.F.);
#8718=ORIENTED_EDGE('',*,*,#6461,.F.);
#8719=ORIENTED_EDGE('',*,*,#6462,.F.);
#8720=ORIENTED_EDGE('',*,*,#6463,.F.);
#8721=ORIENTED_EDGE('',*,*,#6323,.F.);
#8722=ORIENTED_EDGE('',*,*,#6464,.F.);
#8723=ORIENTED_EDGE('',*,*,#6465,.F.);
#8724=ORIENTED_EDGE('',*,*,#6466,.F.);
#8725=ORIENTED_EDGE('',*,*,#6467,.F.);
#8726=ORIENTED_EDGE('',*,*,#6468,.F.);
#8727=ORIENTED_EDGE('',*,*,#6469,.F.);
#8728=ORIENTED_EDGE('',*,*,#6470,.F.);
#8729=ORIENTED_EDGE('',*,*,#6471,.F.);
#8730=ORIENTED_EDGE('',*,*,#6472,.F.);
#8731=ORIENTED_EDGE('',*,*,#6473,.F.);
#8732=ORIENTED_EDGE('',*,*,#6474,.F.);
#8733=ORIENTED_EDGE('',*,*,#6475,.F.);
#8734=ORIENTED_EDGE('',*,*,#6476,.F.);
#8735=ORIENTED_EDGE('',*,*,#6477,.F.);
#8736=ORIENTED_EDGE('',*,*,#6478,.F.);
#8737=ORIENTED_EDGE('',*,*,#6479,.F.);
#8738=ORIENTED_EDGE('',*,*,#6480,.F.);
#8739=ORIENTED_EDGE('',*,*,#6481,.F.);
#8740=ORIENTED_EDGE('',*,*,#6482,.F.);
#8741=ORIENTED_EDGE('',*,*,#6483,.F.);
#8742=ORIENTED_EDGE('',*,*,#6484,.F.);
#8743=ORIENTED_EDGE('',*,*,#6485,.F.);
#8744=ORIENTED_EDGE('',*,*,#6486,.F.);
#8745=ORIENTED_EDGE('',*,*,#6487,.F.);
#8746=ORIENTED_EDGE('',*,*,#6488,.F.);
#8747=ORIENTED_EDGE('',*,*,#6489,.F.);
#8748=ORIENTED_EDGE('',*,*,#6490,.F.);
#8749=ORIENTED_EDGE('',*,*,#6491,.F.);
#8750=ORIENTED_EDGE('',*,*,#6492,.F.);
#8751=ORIENTED_EDGE('',*,*,#6493,.F.);
#8752=ORIENTED_EDGE('',*,*,#6494,.F.);
#8753=ORIENTED_EDGE('',*,*,#6495,.F.);
#8754=ORIENTED_EDGE('',*,*,#6496,.F.);
#8755=ORIENTED_EDGE('',*,*,#6497,.F.);
#8756=ORIENTED_EDGE('',*,*,#6498,.F.);
#8757=ORIENTED_EDGE('',*,*,#6499,.F.);
#8758=ORIENTED_EDGE('',*,*,#6500,.F.);
#8759=ORIENTED_EDGE('',*,*,#6501,.F.);
#8760=ORIENTED_EDGE('',*,*,#6502,.F.);
#8761=ORIENTED_EDGE('',*,*,#6503,.F.);
#8762=ORIENTED_EDGE('',*,*,#6504,.F.);
#8763=ORIENTED_EDGE('',*,*,#6505,.F.);
#8764=ORIENTED_EDGE('',*,*,#6506,.F.);
#8765=ORIENTED_EDGE('',*,*,#6507,.F.);
#8766=ORIENTED_EDGE('',*,*,#6508,.F.);
#8767=ORIENTED_EDGE('',*,*,#6509,.F.);
#8768=ORIENTED_EDGE('',*,*,#6510,.F.);
#8769=ORIENTED_EDGE('',*,*,#6511,.F.);
#8770=ORIENTED_EDGE('',*,*,#6512,.F.);
#8771=ORIENTED_EDGE('',*,*,#6513,.F.);
#8772=ORIENTED_EDGE('',*,*,#6514,.F.);
#8773=ORIENTED_EDGE('',*,*,#6515,.F.);
#8774=ORIENTED_EDGE('',*,*,#6516,.F.);
#8775=ORIENTED_EDGE('',*,*,#6517,.F.);
#8776=ORIENTED_EDGE('',*,*,#6518,.F.);
#8777=ORIENTED_EDGE('',*,*,#6519,.F.);
#8778=ORIENTED_EDGE('',*,*,#6520,.F.);
#8779=ORIENTED_EDGE('',*,*,#6521,.F.);
#8780=ORIENTED_EDGE('',*,*,#6522,.F.);
#8781=ORIENTED_EDGE('',*,*,#6523,.F.);
#8782=ORIENTED_EDGE('',*,*,#6524,.F.);
#8783=ORIENTED_EDGE('',*,*,#6525,.F.);
#8784=ORIENTED_EDGE('',*,*,#6526,.F.);
#8785=ORIENTED_EDGE('',*,*,#6527,.F.);
#8786=ORIENTED_EDGE('',*,*,#6528,.F.);
#8787=ORIENTED_EDGE('',*,*,#6529,.F.);
#8788=ORIENTED_EDGE('',*,*,#6530,.F.);
#8789=ORIENTED_EDGE('',*,*,#6531,.F.);
#8790=ORIENTED_EDGE('',*,*,#6532,.F.);
#8791=ORIENTED_EDGE('',*,*,#6533,.F.);
#8792=ORIENTED_EDGE('',*,*,#6534,.F.);
#8793=ORIENTED_EDGE('',*,*,#6535,.F.);
#8794=ORIENTED_EDGE('',*,*,#6536,.F.);
#8795=ORIENTED_EDGE('',*,*,#6537,.F.);
#8796=ORIENTED_EDGE('',*,*,#6538,.F.);
#8797=ORIENTED_EDGE('',*,*,#6539,.F.);
#8798=ORIENTED_EDGE('',*,*,#6540,.F.);
#8799=ORIENTED_EDGE('',*,*,#6541,.F.);
#8800=ORIENTED_EDGE('',*,*,#6542,.F.);
#8801=ORIENTED_EDGE('',*,*,#6543,.F.);
#8802=ORIENTED_EDGE('',*,*,#6544,.F.);
#8803=ORIENTED_EDGE('',*,*,#6545,.F.);
#8804=ORIENTED_EDGE('',*,*,#6546,.F.);
#8805=ORIENTED_EDGE('',*,*,#6547,.F.);
#8806=ORIENTED_EDGE('',*,*,#6548,.F.);
#8807=ORIENTED_EDGE('',*,*,#6549,.F.);
#8808=ORIENTED_EDGE('',*,*,#6550,.F.);
#8809=ORIENTED_EDGE('',*,*,#6551,.F.);
#8810=ORIENTED_EDGE('',*,*,#6552,.F.);
#8811=ORIENTED_EDGE('',*,*,#6553,.F.);
#8812=ORIENTED_EDGE('',*,*,#6554,.F.);
#8813=ORIENTED_EDGE('',*,*,#6555,.F.);
#8814=ORIENTED_EDGE('',*,*,#6556,.F.);
#8815=ORIENTED_EDGE('',*,*,#6557,.F.);
#8816=ORIENTED_EDGE('',*,*,#6558,.F.);
#8817=ORIENTED_EDGE('',*,*,#6559,.F.);
#8818=ORIENTED_EDGE('',*,*,#6560,.F.);
#8819=ORIENTED_EDGE('',*,*,#6561,.F.);
#8820=ORIENTED_EDGE('',*,*,#6562,.F.);
#8821=ORIENTED_EDGE('',*,*,#6563,.F.);
#8822=ORIENTED_EDGE('',*,*,#6564,.F.);
#8823=ORIENTED_EDGE('',*,*,#6565,.F.);
#8824=ORIENTED_EDGE('',*,*,#6566,.F.);
#8825=ORIENTED_EDGE('',*,*,#6567,.F.);
#8826=ORIENTED_EDGE('',*,*,#6568,.F.);
#8827=ORIENTED_EDGE('',*,*,#6569,.F.);
#8828=ORIENTED_EDGE('',*,*,#6570,.F.);
#8829=ORIENTED_EDGE('',*,*,#6571,.F.);
#8830=ORIENTED_EDGE('',*,*,#6572,.F.);
#8831=ORIENTED_EDGE('',*,*,#6573,.F.);
#8832=ORIENTED_EDGE('',*,*,#6574,.F.);
#8833=ORIENTED_EDGE('',*,*,#6575,.F.);
#8834=ORIENTED_EDGE('',*,*,#6576,.F.);
#8835=ORIENTED_EDGE('',*,*,#6577,.F.);
#8836=ORIENTED_EDGE('',*,*,#6578,.F.);
#8837=ORIENTED_EDGE('',*,*,#6579,.F.);
#8838=ORIENTED_EDGE('',*,*,#6580,.F.);
#8839=ORIENTED_EDGE('',*,*,#6581,.F.);
#8840=ORIENTED_EDGE('',*,*,#6582,.F.);
#8841=ORIENTED_EDGE('',*,*,#6583,.F.);
#8842=ORIENTED_EDGE('',*,*,#6584,.F.);
#8843=ORIENTED_EDGE('',*,*,#6585,.F.);
#8844=ORIENTED_EDGE('',*,*,#6586,.F.);
#8845=ORIENTED_EDGE('',*,*,#6587,.F.);
#8846=ORIENTED_EDGE('',*,*,#6588,.F.);
#8847=ORIENTED_EDGE('',*,*,#6589,.F.);
#8848=ORIENTED_EDGE('',*,*,#6590,.F.);
#8849=ORIENTED_EDGE('',*,*,#6591,.F.);
#8850=ORIENTED_EDGE('',*,*,#6592,.F.);
#8851=ORIENTED_EDGE('',*,*,#6593,.F.);
#8852=ORIENTED_EDGE('',*,*,#6594,.F.);
#8853=ORIENTED_EDGE('',*,*,#6595,.F.);
#8854=ORIENTED_EDGE('',*,*,#6596,.F.);
#8855=ORIENTED_EDGE('',*,*,#6597,.F.);
#8856=ORIENTED_EDGE('',*,*,#6598,.F.);
#8857=ORIENTED_EDGE('',*,*,#6599,.F.);
#8858=ORIENTED_EDGE('',*,*,#6600,.F.);
#8859=ORIENTED_EDGE('',*,*,#6601,.F.);
#8860=ORIENTED_EDGE('',*,*,#6602,.F.);
#8861=ORIENTED_EDGE('',*,*,#6603,.F.);
#8862=ORIENTED_EDGE('',*,*,#6604,.F.);
#8863=ORIENTED_EDGE('',*,*,#6605,.F.);
#8864=ORIENTED_EDGE('',*,*,#6606,.T.);
#8865=ORIENTED_EDGE('',*,*,#6607,.T.);
#8866=ORIENTED_EDGE('',*,*,#6608,.T.);
#8867=ORIENTED_EDGE('',*,*,#6609,.T.);
#8868=ORIENTED_EDGE('',*,*,#6610,.T.);
#8869=ORIENTED_EDGE('',*,*,#6611,.T.);
#8870=ORIENTED_EDGE('',*,*,#6612,.T.);
#8871=ORIENTED_EDGE('',*,*,#6613,.T.);
#8872=ORIENTED_EDGE('',*,*,#6614,.T.);
#8873=ORIENTED_EDGE('',*,*,#6615,.T.);
#8874=ORIENTED_EDGE('',*,*,#6616,.T.);
#8875=ORIENTED_EDGE('',*,*,#6617,.T.);
#8876=ORIENTED_EDGE('',*,*,#6618,.T.);
#8877=ORIENTED_EDGE('',*,*,#6619,.T.);
#8878=ORIENTED_EDGE('',*,*,#6620,.T.);
#8879=ORIENTED_EDGE('',*,*,#6621,.T.);
#8880=ORIENTED_EDGE('',*,*,#6622,.T.);
#8881=ORIENTED_EDGE('',*,*,#6623,.T.);
#8882=ORIENTED_EDGE('',*,*,#6624,.T.);
#8883=ORIENTED_EDGE('',*,*,#6625,.T.);
#8884=ORIENTED_EDGE('',*,*,#6626,.T.);
#8885=ORIENTED_EDGE('',*,*,#6627,.T.);
#8886=ORIENTED_EDGE('',*,*,#6628,.T.);
#8887=ORIENTED_EDGE('',*,*,#6629,.T.);
#8888=ORIENTED_EDGE('',*,*,#6630,.T.);
#8889=ORIENTED_EDGE('',*,*,#6631,.T.);
#8890=ORIENTED_EDGE('',*,*,#6632,.T.);
#8891=ORIENTED_EDGE('',*,*,#6633,.T.);
#8892=ORIENTED_EDGE('',*,*,#6634,.T.);
#8893=ORIENTED_EDGE('',*,*,#6635,.T.);
#8894=ORIENTED_EDGE('',*,*,#6636,.T.);
#8895=ORIENTED_EDGE('',*,*,#6637,.T.);
#8896=ORIENTED_EDGE('',*,*,#6638,.T.);
#8897=ORIENTED_EDGE('',*,*,#6639,.T.);
#8898=ORIENTED_EDGE('',*,*,#6640,.T.);
#8899=ORIENTED_EDGE('',*,*,#6641,.T.);
#8900=ORIENTED_EDGE('',*,*,#6325,.T.);
#8901=ORIENTED_EDGE('',*,*,#6642,.T.);
#8902=ORIENTED_EDGE('',*,*,#6643,.T.);
#8903=ORIENTED_EDGE('',*,*,#6644,.T.);
#8904=ORIENTED_EDGE('',*,*,#6645,.T.);
#8905=ORIENTED_EDGE('',*,*,#6646,.T.);
#8906=ORIENTED_EDGE('',*,*,#6647,.T.);
#8907=ORIENTED_EDGE('',*,*,#6648,.T.);
#8908=ORIENTED_EDGE('',*,*,#6649,.T.);
#8909=ORIENTED_EDGE('',*,*,#6650,.T.);
#8910=ORIENTED_EDGE('',*,*,#6651,.T.);
#8911=ORIENTED_EDGE('',*,*,#6652,.T.);
#8912=ORIENTED_EDGE('',*,*,#6490,.T.);
#8913=ORIENTED_EDGE('',*,*,#6653,.F.);
#8914=ORIENTED_EDGE('',*,*,#6327,.F.);
#8915=ORIENTED_EDGE('',*,*,#6654,.T.);
#8916=ORIENTED_EDGE('',*,*,#6605,.T.);
#8917=ORIENTED_EDGE('',*,*,#6655,.F.);
#8918=ORIENTED_EDGE('',*,*,#6328,.F.);
#8919=ORIENTED_EDGE('',*,*,#6653,.T.);
#8920=ORIENTED_EDGE('',*,*,#6604,.T.);
#8921=ORIENTED_EDGE('',*,*,#6656,.F.);
#8922=ORIENTED_EDGE('',*,*,#6329,.F.);
#8923=ORIENTED_EDGE('',*,*,#6655,.T.);
#8924=ORIENTED_EDGE('',*,*,#6603,.T.);
#8925=ORIENTED_EDGE('',*,*,#6657,.F.);
#8926=ORIENTED_EDGE('',*,*,#6330,.F.);
#8927=ORIENTED_EDGE('',*,*,#6656,.T.);
#8928=ORIENTED_EDGE('',*,*,#6602,.T.);
#8929=ORIENTED_EDGE('',*,*,#6658,.F.);
#8930=ORIENTED_EDGE('',*,*,#6331,.F.);
#8931=ORIENTED_EDGE('',*,*,#6657,.T.);
#8932=ORIENTED_EDGE('',*,*,#6601,.T.);
#8933=ORIENTED_EDGE('',*,*,#6659,.F.);
#8934=ORIENTED_EDGE('',*,*,#6332,.F.);
#8935=ORIENTED_EDGE('',*,*,#6658,.T.);
#8936=ORIENTED_EDGE('',*,*,#6600,.T.);
#8937=ORIENTED_EDGE('',*,*,#6660,.F.);
#8938=ORIENTED_EDGE('',*,*,#6333,.F.);
#8939=ORIENTED_EDGE('',*,*,#6659,.T.);
#8940=ORIENTED_EDGE('',*,*,#6599,.T.);
#8941=ORIENTED_EDGE('',*,*,#6661,.F.);
#8942=ORIENTED_EDGE('',*,*,#6334,.F.);
#8943=ORIENTED_EDGE('',*,*,#6660,.T.);
#8944=ORIENTED_EDGE('',*,*,#6598,.T.);
#8945=ORIENTED_EDGE('',*,*,#6662,.F.);
#8946=ORIENTED_EDGE('',*,*,#6335,.F.);
#8947=ORIENTED_EDGE('',*,*,#6661,.T.);
#8948=ORIENTED_EDGE('',*,*,#6597,.T.);
#8949=ORIENTED_EDGE('',*,*,#6663,.F.);
#8950=ORIENTED_EDGE('',*,*,#6336,.F.);
#8951=ORIENTED_EDGE('',*,*,#6662,.T.);
#8952=ORIENTED_EDGE('',*,*,#6596,.T.);
#8953=ORIENTED_EDGE('',*,*,#6664,.F.);
#8954=ORIENTED_EDGE('',*,*,#6337,.F.);
#8955=ORIENTED_EDGE('',*,*,#6663,.T.);
#8956=ORIENTED_EDGE('',*,*,#6595,.T.);
#8957=ORIENTED_EDGE('',*,*,#6665,.F.);
#8958=ORIENTED_EDGE('',*,*,#6338,.F.);
#8959=ORIENTED_EDGE('',*,*,#6664,.T.);
#8960=ORIENTED_EDGE('',*,*,#6594,.T.);
#8961=ORIENTED_EDGE('',*,*,#6666,.F.);
#8962=ORIENTED_EDGE('',*,*,#6339,.F.);
#8963=ORIENTED_EDGE('',*,*,#6665,.T.);
#8964=ORIENTED_EDGE('',*,*,#6593,.T.);
#8965=ORIENTED_EDGE('',*,*,#6667,.F.);
#8966=ORIENTED_EDGE('',*,*,#6340,.F.);
#8967=ORIENTED_EDGE('',*,*,#6666,.T.);
#8968=ORIENTED_EDGE('',*,*,#6592,.T.);
#8969=ORIENTED_EDGE('',*,*,#6668,.F.);
#8970=ORIENTED_EDGE('',*,*,#6341,.F.);
#8971=ORIENTED_EDGE('',*,*,#6667,.T.);
#8972=ORIENTED_EDGE('',*,*,#6591,.T.);
#8973=ORIENTED_EDGE('',*,*,#6669,.F.);
#8974=ORIENTED_EDGE('',*,*,#6342,.F.);
#8975=ORIENTED_EDGE('',*,*,#6668,.T.);
#8976=ORIENTED_EDGE('',*,*,#6590,.T.);
#8977=ORIENTED_EDGE('',*,*,#6670,.F.);
#8978=ORIENTED_EDGE('',*,*,#6343,.F.);
#8979=ORIENTED_EDGE('',*,*,#6669,.T.);
#8980=ORIENTED_EDGE('',*,*,#6589,.T.);
#8981=ORIENTED_EDGE('',*,*,#6671,.F.);
#8982=ORIENTED_EDGE('',*,*,#6344,.F.);
#8983=ORIENTED_EDGE('',*,*,#6670,.T.);
#8984=ORIENTED_EDGE('',*,*,#6588,.T.);
#8985=ORIENTED_EDGE('',*,*,#6672,.F.);
#8986=ORIENTED_EDGE('',*,*,#6345,.F.);
#8987=ORIENTED_EDGE('',*,*,#6671,.T.);
#8988=ORIENTED_EDGE('',*,*,#6587,.T.);
#8989=ORIENTED_EDGE('',*,*,#6673,.F.);
#8990=ORIENTED_EDGE('',*,*,#6346,.F.);
#8991=ORIENTED_EDGE('',*,*,#6672,.T.);
#8992=ORIENTED_EDGE('',*,*,#6586,.T.);
#8993=ORIENTED_EDGE('',*,*,#6674,.F.);
#8994=ORIENTED_EDGE('',*,*,#6347,.F.);
#8995=ORIENTED_EDGE('',*,*,#6673,.T.);
#8996=ORIENTED_EDGE('',*,*,#6585,.T.);
#8997=ORIENTED_EDGE('',*,*,#6675,.F.);
#8998=ORIENTED_EDGE('',*,*,#6348,.F.);
#8999=ORIENTED_EDGE('',*,*,#6674,.T.);
#9000=ORIENTED_EDGE('',*,*,#6584,.T.);
#9001=ORIENTED_EDGE('',*,*,#6676,.F.);
#9002=ORIENTED_EDGE('',*,*,#6349,.F.);
#9003=ORIENTED_EDGE('',*,*,#6675,.T.);
#9004=ORIENTED_EDGE('',*,*,#6583,.T.);
#9005=ORIENTED_EDGE('',*,*,#6677,.F.);
#9006=ORIENTED_EDGE('',*,*,#6350,.F.);
#9007=ORIENTED_EDGE('',*,*,#6676,.T.);
#9008=ORIENTED_EDGE('',*,*,#6582,.T.);
#9009=ORIENTED_EDGE('',*,*,#6678,.F.);
#9010=ORIENTED_EDGE('',*,*,#6351,.F.);
#9011=ORIENTED_EDGE('',*,*,#6677,.T.);
#9012=ORIENTED_EDGE('',*,*,#6581,.T.);
#9013=ORIENTED_EDGE('',*,*,#6679,.F.);
#9014=ORIENTED_EDGE('',*,*,#6352,.F.);
#9015=ORIENTED_EDGE('',*,*,#6678,.T.);
#9016=ORIENTED_EDGE('',*,*,#6580,.T.);
#9017=ORIENTED_EDGE('',*,*,#6680,.F.);
#9018=ORIENTED_EDGE('',*,*,#6353,.F.);
#9019=ORIENTED_EDGE('',*,*,#6679,.T.);
#9020=ORIENTED_EDGE('',*,*,#6579,.T.);
#9021=ORIENTED_EDGE('',*,*,#6681,.F.);
#9022=ORIENTED_EDGE('',*,*,#6354,.F.);
#9023=ORIENTED_EDGE('',*,*,#6680,.T.);
#9024=ORIENTED_EDGE('',*,*,#6578,.T.);
#9025=ORIENTED_EDGE('',*,*,#6682,.F.);
#9026=ORIENTED_EDGE('',*,*,#6355,.F.);
#9027=ORIENTED_EDGE('',*,*,#6681,.T.);
#9028=ORIENTED_EDGE('',*,*,#6577,.T.);
#9029=ORIENTED_EDGE('',*,*,#6683,.F.);
#9030=ORIENTED_EDGE('',*,*,#6356,.F.);
#9031=ORIENTED_EDGE('',*,*,#6682,.T.);
#9032=ORIENTED_EDGE('',*,*,#6576,.T.);
#9033=ORIENTED_EDGE('',*,*,#6684,.F.);
#9034=ORIENTED_EDGE('',*,*,#6357,.F.);
#9035=ORIENTED_EDGE('',*,*,#6683,.T.);
#9036=ORIENTED_EDGE('',*,*,#6575,.T.);
#9037=ORIENTED_EDGE('',*,*,#6685,.F.);
#9038=ORIENTED_EDGE('',*,*,#6358,.F.);
#9039=ORIENTED_EDGE('',*,*,#6684,.T.);
#9040=ORIENTED_EDGE('',*,*,#6574,.T.);
#9041=ORIENTED_EDGE('',*,*,#6686,.F.);
#9042=ORIENTED_EDGE('',*,*,#6359,.F.);
#9043=ORIENTED_EDGE('',*,*,#6685,.T.);
#9044=ORIENTED_EDGE('',*,*,#6573,.T.);
#9045=ORIENTED_EDGE('',*,*,#6687,.F.);
#9046=ORIENTED_EDGE('',*,*,#6360,.F.);
#9047=ORIENTED_EDGE('',*,*,#6686,.T.);
#9048=ORIENTED_EDGE('',*,*,#6572,.T.);
#9049=ORIENTED_EDGE('',*,*,#6688,.F.);
#9050=ORIENTED_EDGE('',*,*,#6361,.F.);
#9051=ORIENTED_EDGE('',*,*,#6687,.T.);
#9052=ORIENTED_EDGE('',*,*,#6571,.T.);
#9053=ORIENTED_EDGE('',*,*,#6689,.F.);
#9054=ORIENTED_EDGE('',*,*,#6362,.F.);
#9055=ORIENTED_EDGE('',*,*,#6688,.T.);
#9056=ORIENTED_EDGE('',*,*,#6570,.T.);
#9057=ORIENTED_EDGE('',*,*,#6690,.F.);
#9058=ORIENTED_EDGE('',*,*,#6363,.F.);
#9059=ORIENTED_EDGE('',*,*,#6689,.T.);
#9060=ORIENTED_EDGE('',*,*,#6569,.T.);
#9061=ORIENTED_EDGE('',*,*,#6691,.F.);
#9062=ORIENTED_EDGE('',*,*,#6364,.F.);
#9063=ORIENTED_EDGE('',*,*,#6690,.T.);
#9064=ORIENTED_EDGE('',*,*,#6568,.T.);
#9065=ORIENTED_EDGE('',*,*,#6692,.F.);
#9066=ORIENTED_EDGE('',*,*,#6365,.F.);
#9067=ORIENTED_EDGE('',*,*,#6691,.T.);
#9068=ORIENTED_EDGE('',*,*,#6567,.T.);
#9069=ORIENTED_EDGE('',*,*,#6693,.F.);
#9070=ORIENTED_EDGE('',*,*,#6366,.F.);
#9071=ORIENTED_EDGE('',*,*,#6692,.T.);
#9072=ORIENTED_EDGE('',*,*,#6566,.T.);
#9073=ORIENTED_EDGE('',*,*,#6694,.F.);
#9074=ORIENTED_EDGE('',*,*,#6367,.F.);
#9075=ORIENTED_EDGE('',*,*,#6693,.T.);
#9076=ORIENTED_EDGE('',*,*,#6565,.T.);
#9077=ORIENTED_EDGE('',*,*,#6695,.F.);
#9078=ORIENTED_EDGE('',*,*,#6368,.F.);
#9079=ORIENTED_EDGE('',*,*,#6694,.T.);
#9080=ORIENTED_EDGE('',*,*,#6564,.T.);
#9081=ORIENTED_EDGE('',*,*,#6696,.F.);
#9082=ORIENTED_EDGE('',*,*,#6369,.F.);
#9083=ORIENTED_EDGE('',*,*,#6695,.T.);
#9084=ORIENTED_EDGE('',*,*,#6563,.T.);
#9085=ORIENTED_EDGE('',*,*,#6697,.F.);
#9086=ORIENTED_EDGE('',*,*,#6370,.F.);
#9087=ORIENTED_EDGE('',*,*,#6696,.T.);
#9088=ORIENTED_EDGE('',*,*,#6562,.T.);
#9089=ORIENTED_EDGE('',*,*,#6698,.F.);
#9090=ORIENTED_EDGE('',*,*,#6371,.F.);
#9091=ORIENTED_EDGE('',*,*,#6697,.T.);
#9092=ORIENTED_EDGE('',*,*,#6561,.T.);
#9093=ORIENTED_EDGE('',*,*,#6699,.F.);
#9094=ORIENTED_EDGE('',*,*,#6372,.F.);
#9095=ORIENTED_EDGE('',*,*,#6698,.T.);
#9096=ORIENTED_EDGE('',*,*,#6560,.T.);
#9097=ORIENTED_EDGE('',*,*,#6700,.F.);
#9098=ORIENTED_EDGE('',*,*,#6373,.F.);
#9099=ORIENTED_EDGE('',*,*,#6699,.T.);
#9100=ORIENTED_EDGE('',*,*,#6559,.T.);
#9101=ORIENTED_EDGE('',*,*,#6701,.F.);
#9102=ORIENTED_EDGE('',*,*,#6374,.F.);
#9103=ORIENTED_EDGE('',*,*,#6700,.T.);
#9104=ORIENTED_EDGE('',*,*,#6558,.T.);
#9105=ORIENTED_EDGE('',*,*,#6702,.F.);
#9106=ORIENTED_EDGE('',*,*,#6375,.F.);
#9107=ORIENTED_EDGE('',*,*,#6701,.T.);
#9108=ORIENTED_EDGE('',*,*,#6557,.T.);
#9109=ORIENTED_EDGE('',*,*,#6703,.F.);
#9110=ORIENTED_EDGE('',*,*,#6376,.F.);
#9111=ORIENTED_EDGE('',*,*,#6702,.T.);
#9112=ORIENTED_EDGE('',*,*,#6556,.T.);
#9113=ORIENTED_EDGE('',*,*,#6704,.F.);
#9114=ORIENTED_EDGE('',*,*,#6377,.F.);
#9115=ORIENTED_EDGE('',*,*,#6703,.T.);
#9116=ORIENTED_EDGE('',*,*,#6555,.T.);
#9117=ORIENTED_EDGE('',*,*,#6705,.F.);
#9118=ORIENTED_EDGE('',*,*,#6378,.F.);
#9119=ORIENTED_EDGE('',*,*,#6704,.T.);
#9120=ORIENTED_EDGE('',*,*,#6554,.T.);
#9121=ORIENTED_EDGE('',*,*,#6706,.F.);
#9122=ORIENTED_EDGE('',*,*,#6379,.F.);
#9123=ORIENTED_EDGE('',*,*,#6705,.T.);
#9124=ORIENTED_EDGE('',*,*,#6553,.T.);
#9125=ORIENTED_EDGE('',*,*,#6707,.F.);
#9126=ORIENTED_EDGE('',*,*,#6380,.F.);
#9127=ORIENTED_EDGE('',*,*,#6706,.T.);
#9128=ORIENTED_EDGE('',*,*,#6552,.T.);
#9129=ORIENTED_EDGE('',*,*,#6708,.F.);
#9130=ORIENTED_EDGE('',*,*,#6381,.F.);
#9131=ORIENTED_EDGE('',*,*,#6707,.T.);
#9132=ORIENTED_EDGE('',*,*,#6551,.T.);
#9133=ORIENTED_EDGE('',*,*,#6709,.F.);
#9134=ORIENTED_EDGE('',*,*,#6382,.F.);
#9135=ORIENTED_EDGE('',*,*,#6708,.T.);
#9136=ORIENTED_EDGE('',*,*,#6550,.T.);
#9137=ORIENTED_EDGE('',*,*,#6710,.F.);
#9138=ORIENTED_EDGE('',*,*,#6383,.F.);
#9139=ORIENTED_EDGE('',*,*,#6709,.T.);
#9140=ORIENTED_EDGE('',*,*,#6549,.T.);
#9141=ORIENTED_EDGE('',*,*,#6711,.F.);
#9142=ORIENTED_EDGE('',*,*,#6384,.F.);
#9143=ORIENTED_EDGE('',*,*,#6710,.T.);
#9144=ORIENTED_EDGE('',*,*,#6548,.T.);
#9145=ORIENTED_EDGE('',*,*,#6712,.F.);
#9146=ORIENTED_EDGE('',*,*,#6385,.F.);
#9147=ORIENTED_EDGE('',*,*,#6711,.T.);
#9148=ORIENTED_EDGE('',*,*,#6547,.T.);
#9149=ORIENTED_EDGE('',*,*,#6713,.F.);
#9150=ORIENTED_EDGE('',*,*,#6386,.F.);
#9151=ORIENTED_EDGE('',*,*,#6712,.T.);
#9152=ORIENTED_EDGE('',*,*,#6546,.T.);
#9153=ORIENTED_EDGE('',*,*,#6714,.F.);
#9154=ORIENTED_EDGE('',*,*,#6387,.F.);
#9155=ORIENTED_EDGE('',*,*,#6713,.T.);
#9156=ORIENTED_EDGE('',*,*,#6545,.T.);
#9157=ORIENTED_EDGE('',*,*,#6715,.F.);
#9158=ORIENTED_EDGE('',*,*,#6388,.F.);
#9159=ORIENTED_EDGE('',*,*,#6714,.T.);
#9160=ORIENTED_EDGE('',*,*,#6544,.T.);
#9161=ORIENTED_EDGE('',*,*,#6716,.F.);
#9162=ORIENTED_EDGE('',*,*,#6389,.F.);
#9163=ORIENTED_EDGE('',*,*,#6715,.T.);
#9164=ORIENTED_EDGE('',*,*,#6543,.T.);
#9165=ORIENTED_EDGE('',*,*,#6717,.F.);
#9166=ORIENTED_EDGE('',*,*,#6390,.F.);
#9167=ORIENTED_EDGE('',*,*,#6716,.T.);
#9168=ORIENTED_EDGE('',*,*,#6542,.T.);
#9169=ORIENTED_EDGE('',*,*,#6718,.F.);
#9170=ORIENTED_EDGE('',*,*,#6391,.F.);
#9171=ORIENTED_EDGE('',*,*,#6717,.T.);
#9172=ORIENTED_EDGE('',*,*,#6541,.T.);
#9173=ORIENTED_EDGE('',*,*,#6719,.F.);
#9174=ORIENTED_EDGE('',*,*,#6392,.F.);
#9175=ORIENTED_EDGE('',*,*,#6718,.T.);
#9176=ORIENTED_EDGE('',*,*,#6540,.T.);
#9177=ORIENTED_EDGE('',*,*,#6720,.F.);
#9178=ORIENTED_EDGE('',*,*,#6393,.F.);
#9179=ORIENTED_EDGE('',*,*,#6719,.T.);
#9180=ORIENTED_EDGE('',*,*,#6539,.T.);
#9181=ORIENTED_EDGE('',*,*,#6721,.F.);
#9182=ORIENTED_EDGE('',*,*,#6394,.F.);
#9183=ORIENTED_EDGE('',*,*,#6720,.T.);
#9184=ORIENTED_EDGE('',*,*,#6538,.T.);
#9185=ORIENTED_EDGE('',*,*,#6722,.F.);
#9186=ORIENTED_EDGE('',*,*,#6395,.F.);
#9187=ORIENTED_EDGE('',*,*,#6721,.T.);
#9188=ORIENTED_EDGE('',*,*,#6537,.T.);
#9189=ORIENTED_EDGE('',*,*,#6723,.F.);
#9190=ORIENTED_EDGE('',*,*,#6396,.F.);
#9191=ORIENTED_EDGE('',*,*,#6722,.T.);
#9192=ORIENTED_EDGE('',*,*,#6536,.T.);
#9193=ORIENTED_EDGE('',*,*,#6724,.F.);
#9194=ORIENTED_EDGE('',*,*,#6397,.F.);
#9195=ORIENTED_EDGE('',*,*,#6723,.T.);
#9196=ORIENTED_EDGE('',*,*,#6535,.T.);
#9197=ORIENTED_EDGE('',*,*,#6725,.F.);
#9198=ORIENTED_EDGE('',*,*,#6398,.F.);
#9199=ORIENTED_EDGE('',*,*,#6724,.T.);
#9200=ORIENTED_EDGE('',*,*,#6534,.T.);
#9201=ORIENTED_EDGE('',*,*,#6726,.F.);
#9202=ORIENTED_EDGE('',*,*,#6399,.F.);
#9203=ORIENTED_EDGE('',*,*,#6725,.T.);
#9204=ORIENTED_EDGE('',*,*,#6533,.T.);
#9205=ORIENTED_EDGE('',*,*,#6727,.F.);
#9206=ORIENTED_EDGE('',*,*,#6400,.F.);
#9207=ORIENTED_EDGE('',*,*,#6726,.T.);
#9208=ORIENTED_EDGE('',*,*,#6532,.T.);
#9209=ORIENTED_EDGE('',*,*,#6728,.F.);
#9210=ORIENTED_EDGE('',*,*,#6401,.F.);
#9211=ORIENTED_EDGE('',*,*,#6727,.T.);
#9212=ORIENTED_EDGE('',*,*,#6531,.T.);
#9213=ORIENTED_EDGE('',*,*,#6729,.F.);
#9214=ORIENTED_EDGE('',*,*,#6402,.F.);
#9215=ORIENTED_EDGE('',*,*,#6728,.T.);
#9216=ORIENTED_EDGE('',*,*,#6530,.T.);
#9217=ORIENTED_EDGE('',*,*,#6730,.F.);
#9218=ORIENTED_EDGE('',*,*,#6403,.F.);
#9219=ORIENTED_EDGE('',*,*,#6729,.T.);
#9220=ORIENTED_EDGE('',*,*,#6529,.T.);
#9221=ORIENTED_EDGE('',*,*,#6731,.F.);
#9222=ORIENTED_EDGE('',*,*,#6404,.F.);
#9223=ORIENTED_EDGE('',*,*,#6730,.T.);
#9224=ORIENTED_EDGE('',*,*,#6528,.T.);
#9225=ORIENTED_EDGE('',*,*,#6732,.F.);
#9226=ORIENTED_EDGE('',*,*,#6405,.F.);
#9227=ORIENTED_EDGE('',*,*,#6731,.T.);
#9228=ORIENTED_EDGE('',*,*,#6527,.T.);
#9229=ORIENTED_EDGE('',*,*,#6733,.F.);
#9230=ORIENTED_EDGE('',*,*,#6406,.F.);
#9231=ORIENTED_EDGE('',*,*,#6732,.T.);
#9232=ORIENTED_EDGE('',*,*,#6526,.T.);
#9233=ORIENTED_EDGE('',*,*,#6734,.F.);
#9234=ORIENTED_EDGE('',*,*,#6407,.F.);
#9235=ORIENTED_EDGE('',*,*,#6733,.T.);
#9236=ORIENTED_EDGE('',*,*,#6525,.T.);
#9237=ORIENTED_EDGE('',*,*,#6735,.F.);
#9238=ORIENTED_EDGE('',*,*,#6408,.F.);
#9239=ORIENTED_EDGE('',*,*,#6734,.T.);
#9240=ORIENTED_EDGE('',*,*,#6524,.T.);
#9241=ORIENTED_EDGE('',*,*,#6736,.F.);
#9242=ORIENTED_EDGE('',*,*,#6409,.F.);
#9243=ORIENTED_EDGE('',*,*,#6735,.T.);
#9244=ORIENTED_EDGE('',*,*,#6523,.T.);
#9245=ORIENTED_EDGE('',*,*,#6737,.F.);
#9246=ORIENTED_EDGE('',*,*,#6410,.F.);
#9247=ORIENTED_EDGE('',*,*,#6736,.T.);
#9248=ORIENTED_EDGE('',*,*,#6522,.T.);
#9249=ORIENTED_EDGE('',*,*,#6738,.F.);
#9250=ORIENTED_EDGE('',*,*,#6411,.F.);
#9251=ORIENTED_EDGE('',*,*,#6737,.T.);
#9252=ORIENTED_EDGE('',*,*,#6521,.T.);
#9253=ORIENTED_EDGE('',*,*,#6739,.F.);
#9254=ORIENTED_EDGE('',*,*,#6412,.F.);
#9255=ORIENTED_EDGE('',*,*,#6738,.T.);
#9256=ORIENTED_EDGE('',*,*,#6520,.T.);
#9257=ORIENTED_EDGE('',*,*,#6740,.F.);
#9258=ORIENTED_EDGE('',*,*,#6413,.F.);
#9259=ORIENTED_EDGE('',*,*,#6739,.T.);
#9260=ORIENTED_EDGE('',*,*,#6519,.T.);
#9261=ORIENTED_EDGE('',*,*,#6741,.F.);
#9262=ORIENTED_EDGE('',*,*,#6414,.F.);
#9263=ORIENTED_EDGE('',*,*,#6740,.T.);
#9264=ORIENTED_EDGE('',*,*,#6518,.T.);
#9265=ORIENTED_EDGE('',*,*,#6742,.F.);
#9266=ORIENTED_EDGE('',*,*,#6415,.F.);
#9267=ORIENTED_EDGE('',*,*,#6741,.T.);
#9268=ORIENTED_EDGE('',*,*,#6517,.T.);
#9269=ORIENTED_EDGE('',*,*,#6743,.F.);
#9270=ORIENTED_EDGE('',*,*,#6416,.F.);
#9271=ORIENTED_EDGE('',*,*,#6742,.T.);
#9272=ORIENTED_EDGE('',*,*,#6516,.T.);
#9273=ORIENTED_EDGE('',*,*,#6744,.F.);
#9274=ORIENTED_EDGE('',*,*,#6417,.F.);
#9275=ORIENTED_EDGE('',*,*,#6743,.T.);
#9276=ORIENTED_EDGE('',*,*,#6515,.T.);
#9277=ORIENTED_EDGE('',*,*,#6745,.F.);
#9278=ORIENTED_EDGE('',*,*,#6418,.F.);
#9279=ORIENTED_EDGE('',*,*,#6744,.T.);
#9280=ORIENTED_EDGE('',*,*,#6514,.T.);
#9281=ORIENTED_EDGE('',*,*,#6746,.F.);
#9282=ORIENTED_EDGE('',*,*,#6419,.F.);
#9283=ORIENTED_EDGE('',*,*,#6745,.T.);
#9284=ORIENTED_EDGE('',*,*,#6513,.T.);
#9285=ORIENTED_EDGE('',*,*,#6747,.F.);
#9286=ORIENTED_EDGE('',*,*,#6420,.F.);
#9287=ORIENTED_EDGE('',*,*,#6746,.T.);
#9288=ORIENTED_EDGE('',*,*,#6512,.T.);
#9289=ORIENTED_EDGE('',*,*,#6748,.F.);
#9290=ORIENTED_EDGE('',*,*,#6421,.F.);
#9291=ORIENTED_EDGE('',*,*,#6747,.T.);
#9292=ORIENTED_EDGE('',*,*,#6511,.T.);
#9293=ORIENTED_EDGE('',*,*,#6749,.F.);
#9294=ORIENTED_EDGE('',*,*,#6422,.F.);
#9295=ORIENTED_EDGE('',*,*,#6748,.T.);
#9296=ORIENTED_EDGE('',*,*,#6510,.T.);
#9297=ORIENTED_EDGE('',*,*,#6750,.F.);
#9298=ORIENTED_EDGE('',*,*,#6423,.F.);
#9299=ORIENTED_EDGE('',*,*,#6749,.T.);
#9300=ORIENTED_EDGE('',*,*,#6509,.T.);
#9301=ORIENTED_EDGE('',*,*,#6751,.F.);
#9302=ORIENTED_EDGE('',*,*,#6424,.F.);
#9303=ORIENTED_EDGE('',*,*,#6750,.T.);
#9304=ORIENTED_EDGE('',*,*,#6508,.T.);
#9305=ORIENTED_EDGE('',*,*,#6752,.F.);
#9306=ORIENTED_EDGE('',*,*,#6425,.F.);
#9307=ORIENTED_EDGE('',*,*,#6751,.T.);
#9308=ORIENTED_EDGE('',*,*,#6507,.T.);
#9309=ORIENTED_EDGE('',*,*,#6753,.F.);
#9310=ORIENTED_EDGE('',*,*,#6426,.F.);
#9311=ORIENTED_EDGE('',*,*,#6752,.T.);
#9312=ORIENTED_EDGE('',*,*,#6506,.T.);
#9313=ORIENTED_EDGE('',*,*,#6754,.F.);
#9314=ORIENTED_EDGE('',*,*,#6427,.F.);
#9315=ORIENTED_EDGE('',*,*,#6753,.T.);
#9316=ORIENTED_EDGE('',*,*,#6505,.T.);
#9317=ORIENTED_EDGE('',*,*,#6755,.F.);
#9318=ORIENTED_EDGE('',*,*,#6428,.F.);
#9319=ORIENTED_EDGE('',*,*,#6754,.T.);
#9320=ORIENTED_EDGE('',*,*,#6504,.T.);
#9321=ORIENTED_EDGE('',*,*,#6756,.F.);
#9322=ORIENTED_EDGE('',*,*,#6429,.F.);
#9323=ORIENTED_EDGE('',*,*,#6755,.T.);
#9324=ORIENTED_EDGE('',*,*,#6503,.T.);
#9325=ORIENTED_EDGE('',*,*,#6757,.F.);
#9326=ORIENTED_EDGE('',*,*,#6430,.F.);
#9327=ORIENTED_EDGE('',*,*,#6756,.T.);
#9328=ORIENTED_EDGE('',*,*,#6502,.T.);
#9329=ORIENTED_EDGE('',*,*,#6758,.F.);
#9330=ORIENTED_EDGE('',*,*,#6431,.F.);
#9331=ORIENTED_EDGE('',*,*,#6757,.T.);
#9332=ORIENTED_EDGE('',*,*,#6501,.T.);
#9333=ORIENTED_EDGE('',*,*,#6759,.F.);
#9334=ORIENTED_EDGE('',*,*,#6432,.F.);
#9335=ORIENTED_EDGE('',*,*,#6758,.T.);
#9336=ORIENTED_EDGE('',*,*,#6500,.T.);
#9337=ORIENTED_EDGE('',*,*,#6760,.F.);
#9338=ORIENTED_EDGE('',*,*,#6433,.F.);
#9339=ORIENTED_EDGE('',*,*,#6759,.T.);
#9340=ORIENTED_EDGE('',*,*,#6499,.T.);
#9341=ORIENTED_EDGE('',*,*,#6761,.F.);
#9342=ORIENTED_EDGE('',*,*,#6434,.F.);
#9343=ORIENTED_EDGE('',*,*,#6760,.T.);
#9344=ORIENTED_EDGE('',*,*,#6498,.T.);
#9345=ORIENTED_EDGE('',*,*,#6762,.F.);
#9346=ORIENTED_EDGE('',*,*,#6435,.F.);
#9347=ORIENTED_EDGE('',*,*,#6761,.T.);
#9348=ORIENTED_EDGE('',*,*,#6497,.T.);
#9349=ORIENTED_EDGE('',*,*,#6763,.F.);
#9350=ORIENTED_EDGE('',*,*,#6436,.F.);
#9351=ORIENTED_EDGE('',*,*,#6762,.T.);
#9352=ORIENTED_EDGE('',*,*,#6496,.T.);
#9353=ORIENTED_EDGE('',*,*,#6764,.F.);
#9354=ORIENTED_EDGE('',*,*,#6437,.F.);
#9355=ORIENTED_EDGE('',*,*,#6763,.T.);
#9356=ORIENTED_EDGE('',*,*,#6495,.T.);
#9357=ORIENTED_EDGE('',*,*,#6765,.F.);
#9358=ORIENTED_EDGE('',*,*,#6438,.F.);
#9359=ORIENTED_EDGE('',*,*,#6764,.T.);
#9360=ORIENTED_EDGE('',*,*,#6494,.T.);
#9361=ORIENTED_EDGE('',*,*,#6766,.F.);
#9362=ORIENTED_EDGE('',*,*,#6439,.F.);
#9363=ORIENTED_EDGE('',*,*,#6765,.T.);
#9364=ORIENTED_EDGE('',*,*,#6493,.T.);
#9365=ORIENTED_EDGE('',*,*,#6767,.F.);
#9366=ORIENTED_EDGE('',*,*,#6440,.F.);
#9367=ORIENTED_EDGE('',*,*,#6766,.T.);
#9368=ORIENTED_EDGE('',*,*,#6492,.T.);
#9369=ORIENTED_EDGE('',*,*,#6768,.F.);
#9370=ORIENTED_EDGE('',*,*,#6441,.F.);
#9371=ORIENTED_EDGE('',*,*,#6767,.T.);
#9372=ORIENTED_EDGE('',*,*,#6491,.T.);
#9373=ORIENTED_EDGE('',*,*,#6654,.F.);
#9374=ORIENTED_EDGE('',*,*,#6442,.F.);
#9375=ORIENTED_EDGE('',*,*,#6768,.T.);
#9376=ORIENTED_EDGE('',*,*,#6606,.F.);
#9377=ORIENTED_EDGE('',*,*,#6769,.F.);
#9378=ORIENTED_EDGE('',*,*,#6444,.T.);
#9379=ORIENTED_EDGE('',*,*,#6770,.T.);
#9380=ORIENTED_EDGE('',*,*,#6607,.F.);
#9381=ORIENTED_EDGE('',*,*,#6770,.F.);
#9382=ORIENTED_EDGE('',*,*,#6443,.T.);
#9383=ORIENTED_EDGE('',*,*,#6771,.T.);
#9384=ORIENTED_EDGE('',*,*,#6608,.F.);
#9385=ORIENTED_EDGE('',*,*,#6771,.F.);
#9386=ORIENTED_EDGE('',*,*,#6450,.T.);
#9387=ORIENTED_EDGE('',*,*,#6772,.T.);
#9388=ORIENTED_EDGE('',*,*,#6609,.F.);
#9389=ORIENTED_EDGE('',*,*,#6772,.F.);
#9390=ORIENTED_EDGE('',*,*,#6449,.T.);
#9391=ORIENTED_EDGE('',*,*,#6773,.T.);
#9392=ORIENTED_EDGE('',*,*,#6610,.F.);
#9393=ORIENTED_EDGE('',*,*,#6773,.F.);
#9394=ORIENTED_EDGE('',*,*,#6448,.T.);
#9395=ORIENTED_EDGE('',*,*,#6774,.T.);
#9396=ORIENTED_EDGE('',*,*,#6611,.F.);
#9397=ORIENTED_EDGE('',*,*,#6774,.F.);
#9398=ORIENTED_EDGE('',*,*,#6447,.T.);
#9399=ORIENTED_EDGE('',*,*,#6775,.T.);
#9400=ORIENTED_EDGE('',*,*,#6612,.F.);
#9401=ORIENTED_EDGE('',*,*,#6775,.F.);
#9402=ORIENTED_EDGE('',*,*,#6446,.T.);
#9403=ORIENTED_EDGE('',*,*,#6776,.T.);
#9404=ORIENTED_EDGE('',*,*,#6613,.F.);
#9405=ORIENTED_EDGE('',*,*,#6776,.F.);
#9406=ORIENTED_EDGE('',*,*,#6445,.T.);
#9407=ORIENTED_EDGE('',*,*,#6769,.T.);
#9408=ORIENTED_EDGE('',*,*,#6638,.F.);
#9409=ORIENTED_EDGE('',*,*,#6777,.F.);
#9410=ORIENTED_EDGE('',*,*,#6452,.T.);
#9411=ORIENTED_EDGE('',*,*,#6778,.T.);
#9412=ORIENTED_EDGE('',*,*,#6639,.F.);
#9413=ORIENTED_EDGE('',*,*,#6778,.F.);
#9414=ORIENTED_EDGE('',*,*,#6451,.T.);
#9415=ORIENTED_EDGE('',*,*,#6779,.T.);
#9416=ORIENTED_EDGE('',*,*,#6640,.F.);
#9417=ORIENTED_EDGE('',*,*,#6779,.F.);
#9418=ORIENTED_EDGE('',*,*,#6465,.T.);
#9419=ORIENTED_EDGE('',*,*,#6780,.T.);
#9420=ORIENTED_EDGE('',*,*,#6641,.F.);
#9421=ORIENTED_EDGE('',*,*,#6780,.F.);
#9422=ORIENTED_EDGE('',*,*,#6464,.T.);
#9423=ORIENTED_EDGE('',*,*,#6326,.T.);
#9424=ORIENTED_EDGE('',*,*,#6642,.F.);
#9425=ORIENTED_EDGE('',*,*,#6324,.F.);
#9426=ORIENTED_EDGE('',*,*,#6463,.T.);
#9427=ORIENTED_EDGE('',*,*,#6781,.T.);
#9428=ORIENTED_EDGE('',*,*,#6643,.F.);
#9429=ORIENTED_EDGE('',*,*,#6781,.F.);
#9430=ORIENTED_EDGE('',*,*,#6462,.T.);
#9431=ORIENTED_EDGE('',*,*,#6782,.T.);
#9432=ORIENTED_EDGE('',*,*,#6644,.F.);
#9433=ORIENTED_EDGE('',*,*,#6782,.F.);
#9434=ORIENTED_EDGE('',*,*,#6461,.T.);
#9435=ORIENTED_EDGE('',*,*,#6783,.T.);
#9436=ORIENTED_EDGE('',*,*,#6645,.F.);
#9437=ORIENTED_EDGE('',*,*,#6783,.F.);
#9438=ORIENTED_EDGE('',*,*,#6460,.T.);
#9439=ORIENTED_EDGE('',*,*,#6784,.T.);
#9440=ORIENTED_EDGE('',*,*,#6646,.F.);
#9441=ORIENTED_EDGE('',*,*,#6784,.F.);
#9442=ORIENTED_EDGE('',*,*,#6459,.T.);
#9443=ORIENTED_EDGE('',*,*,#6785,.T.);
#9444=ORIENTED_EDGE('',*,*,#6647,.F.);
#9445=ORIENTED_EDGE('',*,*,#6785,.F.);
#9446=ORIENTED_EDGE('',*,*,#6458,.T.);
#9447=ORIENTED_EDGE('',*,*,#6786,.T.);
#9448=ORIENTED_EDGE('',*,*,#6648,.F.);
#9449=ORIENTED_EDGE('',*,*,#6786,.F.);
#9450=ORIENTED_EDGE('',*,*,#6457,.T.);
#9451=ORIENTED_EDGE('',*,*,#6787,.T.);
#9452=ORIENTED_EDGE('',*,*,#6649,.F.);
#9453=ORIENTED_EDGE('',*,*,#6787,.F.);
#9454=ORIENTED_EDGE('',*,*,#6456,.T.);
#9455=ORIENTED_EDGE('',*,*,#6788,.T.);
#9456=ORIENTED_EDGE('',*,*,#6650,.F.);
#9457=ORIENTED_EDGE('',*,*,#6788,.F.);
#9458=ORIENTED_EDGE('',*,*,#6455,.T.);
#9459=ORIENTED_EDGE('',*,*,#6789,.T.);
#9460=ORIENTED_EDGE('',*,*,#6651,.F.);
#9461=ORIENTED_EDGE('',*,*,#6789,.F.);
#9462=ORIENTED_EDGE('',*,*,#6454,.T.);
#9463=ORIENTED_EDGE('',*,*,#6790,.T.);
#9464=ORIENTED_EDGE('',*,*,#6652,.F.);
#9465=ORIENTED_EDGE('',*,*,#6790,.F.);
#9466=ORIENTED_EDGE('',*,*,#6453,.T.);
#9467=ORIENTED_EDGE('',*,*,#6777,.T.);
#9468=ORIENTED_EDGE('',*,*,#6614,.F.);
#9469=ORIENTED_EDGE('',*,*,#6791,.F.);
#9470=ORIENTED_EDGE('',*,*,#6467,.T.);
#9471=ORIENTED_EDGE('',*,*,#6792,.T.);
#9472=ORIENTED_EDGE('',*,*,#6615,.F.);
#9473=ORIENTED_EDGE('',*,*,#6792,.F.);
#9474=ORIENTED_EDGE('',*,*,#6466,.T.);
#9475=ORIENTED_EDGE('',*,*,#6793,.T.);
#9476=ORIENTED_EDGE('',*,*,#6616,.F.);
#9477=ORIENTED_EDGE('',*,*,#6793,.F.);
#9478=ORIENTED_EDGE('',*,*,#6473,.T.);
#9479=ORIENTED_EDGE('',*,*,#6794,.T.);
#9480=ORIENTED_EDGE('',*,*,#6617,.F.);
#9481=ORIENTED_EDGE('',*,*,#6794,.F.);
#9482=ORIENTED_EDGE('',*,*,#6472,.T.);
#9483=ORIENTED_EDGE('',*,*,#6795,.T.);
#9484=ORIENTED_EDGE('',*,*,#6618,.F.);
#9485=ORIENTED_EDGE('',*,*,#6795,.F.);
#9486=ORIENTED_EDGE('',*,*,#6471,.T.);
#9487=ORIENTED_EDGE('',*,*,#6796,.T.);
#9488=ORIENTED_EDGE('',*,*,#6619,.F.);
#9489=ORIENTED_EDGE('',*,*,#6796,.F.);
#9490=ORIENTED_EDGE('',*,*,#6470,.T.);
#9491=ORIENTED_EDGE('',*,*,#6797,.T.);
#9492=ORIENTED_EDGE('',*,*,#6620,.F.);
#9493=ORIENTED_EDGE('',*,*,#6797,.F.);
#9494=ORIENTED_EDGE('',*,*,#6469,.T.);
#9495=ORIENTED_EDGE('',*,*,#6798,.T.);
#9496=ORIENTED_EDGE('',*,*,#6621,.F.);
#9497=ORIENTED_EDGE('',*,*,#6798,.F.);
#9498=ORIENTED_EDGE('',*,*,#6468,.T.);
#9499=ORIENTED_EDGE('',*,*,#6791,.T.);
#9500=ORIENTED_EDGE('',*,*,#6630,.F.);
#9501=ORIENTED_EDGE('',*,*,#6799,.F.);
#9502=ORIENTED_EDGE('',*,*,#6475,.T.);
#9503=ORIENTED_EDGE('',*,*,#6800,.T.);
#9504=ORIENTED_EDGE('',*,*,#6631,.F.);
#9505=ORIENTED_EDGE('',*,*,#6800,.F.);
#9506=ORIENTED_EDGE('',*,*,#6474,.T.);
#9507=ORIENTED_EDGE('',*,*,#6801,.T.);
#9508=ORIENTED_EDGE('',*,*,#6632,.F.);
#9509=ORIENTED_EDGE('',*,*,#6801,.F.);
#9510=ORIENTED_EDGE('',*,*,#6481,.T.);
#9511=ORIENTED_EDGE('',*,*,#6802,.T.);
#9512=ORIENTED_EDGE('',*,*,#6633,.F.);
#9513=ORIENTED_EDGE('',*,*,#6802,.F.);
#9514=ORIENTED_EDGE('',*,*,#6480,.T.);
#9515=ORIENTED_EDGE('',*,*,#6803,.T.);
#9516=ORIENTED_EDGE('',*,*,#6634,.F.);
#9517=ORIENTED_EDGE('',*,*,#6803,.F.);
#9518=ORIENTED_EDGE('',*,*,#6479,.T.);
#9519=ORIENTED_EDGE('',*,*,#6804,.T.);
#9520=ORIENTED_EDGE('',*,*,#6635,.F.);
#9521=ORIENTED_EDGE('',*,*,#6804,.F.);
#9522=ORIENTED_EDGE('',*,*,#6478,.T.);
#9523=ORIENTED_EDGE('',*,*,#6805,.T.);
#9524=ORIENTED_EDGE('',*,*,#6636,.F.);
#9525=ORIENTED_EDGE('',*,*,#6805,.F.);
#9526=ORIENTED_EDGE('',*,*,#6477,.T.);
#9527=ORIENTED_EDGE('',*,*,#6806,.T.);
#9528=ORIENTED_EDGE('',*,*,#6637,.F.);
#9529=ORIENTED_EDGE('',*,*,#6806,.F.);
#9530=ORIENTED_EDGE('',*,*,#6476,.T.);
#9531=ORIENTED_EDGE('',*,*,#6799,.T.);
#9532=ORIENTED_EDGE('',*,*,#6622,.F.);
#9533=ORIENTED_EDGE('',*,*,#6807,.F.);
#9534=ORIENTED_EDGE('',*,*,#6483,.T.);
#9535=ORIENTED_EDGE('',*,*,#6808,.T.);
#9536=ORIENTED_EDGE('',*,*,#6623,.F.);
#9537=ORIENTED_EDGE('',*,*,#6808,.F.);
#9538=ORIENTED_EDGE('',*,*,#6482,.T.);
#9539=ORIENTED_EDGE('',*,*,#6809,.T.);
#9540=ORIENTED_EDGE('',*,*,#6624,.F.);
#9541=ORIENTED_EDGE('',*,*,#6809,.F.);
#9542=ORIENTED_EDGE('',*,*,#6489,.T.);
#9543=ORIENTED_EDGE('',*,*,#6810,.T.);
#9544=ORIENTED_EDGE('',*,*,#6625,.F.);
#9545=ORIENTED_EDGE('',*,*,#6810,.F.);
#9546=ORIENTED_EDGE('',*,*,#6488,.T.);
#9547=ORIENTED_EDGE('',*,*,#6811,.T.);
#9548=ORIENTED_EDGE('',*,*,#6626,.F.);
#9549=ORIENTED_EDGE('',*,*,#6811,.F.);
#9550=ORIENTED_EDGE('',*,*,#6487,.T.);
#9551=ORIENTED_EDGE('',*,*,#6812,.T.);
#9552=ORIENTED_EDGE('',*,*,#6627,.F.);
#9553=ORIENTED_EDGE('',*,*,#6812,.F.);
#9554=ORIENTED_EDGE('',*,*,#6486,.T.);
#9555=ORIENTED_EDGE('',*,*,#6813,.T.);
#9556=ORIENTED_EDGE('',*,*,#6628,.F.);
#9557=ORIENTED_EDGE('',*,*,#6813,.F.);
#9558=ORIENTED_EDGE('',*,*,#6485,.T.);
#9559=ORIENTED_EDGE('',*,*,#6814,.T.);
#9560=ORIENTED_EDGE('',*,*,#6629,.F.);
#9561=ORIENTED_EDGE('',*,*,#6814,.F.);
#9562=ORIENTED_EDGE('',*,*,#6484,.T.);
#9563=ORIENTED_EDGE('',*,*,#6807,.T.);
#9564=ORIENTED_EDGE('',*,*,#6815,.T.);
#9565=ORIENTED_EDGE('',*,*,#6816,.T.);
#9566=ORIENTED_EDGE('',*,*,#6817,.F.);
#9567=ORIENTED_EDGE('',*,*,#6816,.F.);
#9568=ORIENTED_EDGE('',*,*,#6818,.F.);
#9569=ORIENTED_EDGE('',*,*,#6819,.T.);
#9570=ORIENTED_EDGE('',*,*,#6820,.T.);
#9571=ORIENTED_EDGE('',*,*,#6819,.F.);
#9572=ORIENTED_EDGE('',*,*,#6821,.F.);
#9573=ORIENTED_EDGE('',*,*,#6822,.T.);
#9574=ORIENTED_EDGE('',*,*,#6823,.F.);
#9575=ORIENTED_EDGE('',*,*,#6824,.F.);
#9576=ORIENTED_EDGE('',*,*,#6825,.T.);
#9577=ORIENTED_EDGE('',*,*,#6826,.T.);
#9578=ORIENTED_EDGE('',*,*,#6827,.T.);
#9579=ORIENTED_EDGE('',*,*,#6828,.T.);
#9580=ORIENTED_EDGE('',*,*,#6829,.F.);
#9581=ORIENTED_EDGE('',*,*,#6830,.T.);
#9582=ORIENTED_EDGE('',*,*,#6831,.F.);
#9583=ORIENTED_EDGE('',*,*,#6832,.T.);
#9584=ORIENTED_EDGE('',*,*,#6833,.F.);
#9585=ORIENTED_EDGE('',*,*,#6834,.T.);
#9586=ORIENTED_EDGE('',*,*,#6835,.F.);
#9587=ORIENTED_EDGE('',*,*,#6829,.T.);
#9588=ORIENTED_EDGE('',*,*,#6836,.F.);
#9589=ORIENTED_EDGE('',*,*,#6837,.F.);
#9590=ORIENTED_EDGE('',*,*,#6838,.T.);
#9591=ORIENTED_EDGE('',*,*,#6835,.T.);
#9592=ORIENTED_EDGE('',*,*,#6839,.T.);
#9593=ORIENTED_EDGE('',*,*,#6840,.F.);
#9594=ORIENTED_EDGE('',*,*,#6841,.T.);
#9595=ORIENTED_EDGE('',*,*,#6840,.T.);
#9596=ORIENTED_EDGE('',*,*,#6842,.T.);
#9597=ORIENTED_EDGE('',*,*,#6843,.F.);
#9598=ORIENTED_EDGE('',*,*,#6844,.T.);
#9599=ORIENTED_EDGE('',*,*,#6845,.T.);
#9600=ORIENTED_EDGE('',*,*,#6846,.T.);
#9601=ORIENTED_EDGE('',*,*,#6815,.F.);
#9602=ORIENTED_EDGE('',*,*,#6847,.F.);
#9603=ORIENTED_EDGE('',*,*,#6848,.T.);
#9604=ORIENTED_EDGE('',*,*,#6849,.T.);
#9605=ORIENTED_EDGE('',*,*,#6850,.T.);
#9606=ORIENTED_EDGE('',*,*,#6851,.T.);
#9607=ORIENTED_EDGE('',*,*,#6852,.T.);
#9608=ORIENTED_EDGE('',*,*,#6853,.T.);
#9609=ORIENTED_EDGE('',*,*,#6854,.T.);
#9610=ORIENTED_EDGE('',*,*,#6855,.T.);
#9611=ORIENTED_EDGE('',*,*,#6856,.T.);
#9612=ORIENTED_EDGE('',*,*,#6857,.T.);
#9613=ORIENTED_EDGE('',*,*,#6858,.T.);
#9614=ORIENTED_EDGE('',*,*,#6859,.F.);
#9615=ORIENTED_EDGE('',*,*,#6860,.F.);
#9616=ORIENTED_EDGE('',*,*,#6861,.T.);
#9617=ORIENTED_EDGE('',*,*,#6824,.T.);
#9618=ORIENTED_EDGE('',*,*,#6862,.F.);
#9619=ORIENTED_EDGE('',*,*,#6863,.F.);
#9620=ORIENTED_EDGE('',*,*,#6864,.T.);
#9621=ORIENTED_EDGE('',*,*,#6859,.T.);
#9622=ORIENTED_EDGE('',*,*,#6865,.T.);
#9623=ORIENTED_EDGE('',*,*,#6866,.T.);
#9624=ORIENTED_EDGE('',*,*,#6867,.T.);
#9625=ORIENTED_EDGE('',*,*,#6860,.T.);
#9626=ORIENTED_EDGE('',*,*,#6868,.T.);
#9627=ORIENTED_EDGE('',*,*,#6869,.F.);
#9628=ORIENTED_EDGE('',*,*,#6870,.T.);
#9629=ORIENTED_EDGE('',*,*,#6820,.F.);
#9630=ORIENTED_EDGE('',*,*,#6871,.T.);
#9631=ORIENTED_EDGE('',*,*,#6872,.T.);
#9632=ORIENTED_EDGE('',*,*,#6873,.T.);
#9633=ORIENTED_EDGE('',*,*,#6874,.T.);
#9634=ORIENTED_EDGE('',*,*,#6875,.T.);
#9635=ORIENTED_EDGE('',*,*,#6876,.T.);
#9636=ORIENTED_EDGE('',*,*,#6877,.F.);
#9637=ORIENTED_EDGE('',*,*,#6878,.T.);
#9638=ORIENTED_EDGE('',*,*,#6877,.T.);
#9639=ORIENTED_EDGE('',*,*,#6879,.T.);
#9640=ORIENTED_EDGE('',*,*,#6826,.F.);
#9641=ORIENTED_EDGE('',*,*,#6880,.T.);
#9642=ORIENTED_EDGE('',*,*,#6845,.F.);
#9643=ORIENTED_EDGE('',*,*,#6881,.T.);
#9644=ORIENTED_EDGE('',*,*,#6853,.F.);
#9645=ORIENTED_EDGE('',*,*,#6882,.T.);
#9646=ORIENTED_EDGE('',*,*,#6821,.T.);
#9647=ORIENTED_EDGE('',*,*,#6883,.T.);
#9648=ORIENTED_EDGE('',*,*,#6866,.F.);
#9649=ORIENTED_EDGE('',*,*,#6884,.T.);
#9650=ORIENTED_EDGE('',*,*,#6885,.F.);
#9651=ORIENTED_EDGE('',*,*,#6886,.F.);
#9652=ORIENTED_EDGE('',*,*,#6887,.F.);
#9653=ORIENTED_EDGE('',*,*,#6888,.F.);
#9654=ORIENTED_EDGE('',*,*,#6833,.T.);
#9655=ORIENTED_EDGE('',*,*,#6889,.T.);
#9656=ORIENTED_EDGE('',*,*,#6871,.F.);
#9657=ORIENTED_EDGE('',*,*,#6890,.T.);
#9658=ORIENTED_EDGE('',*,*,#6869,.T.);
#9659=ORIENTED_EDGE('',*,*,#6891,.T.);
#9660=ORIENTED_EDGE('',*,*,#6857,.F.);
#9661=ORIENTED_EDGE('',*,*,#6892,.T.);
#9662=ORIENTED_EDGE('',*,*,#6847,.T.);
#9663=ORIENTED_EDGE('',*,*,#6893,.T.);
#9664=ORIENTED_EDGE('',*,*,#6843,.T.);
#9665=ORIENTED_EDGE('',*,*,#6894,.T.);
#9666=ORIENTED_EDGE('',*,*,#6895,.T.);
#9667=ORIENTED_EDGE('',*,*,#6896,.T.);
#9668=ORIENTED_EDGE('',*,*,#6897,.T.);
#9669=ORIENTED_EDGE('',*,*,#6898,.T.);
#9670=ORIENTED_EDGE('',*,*,#6885,.T.);
#9671=ORIENTED_EDGE('',*,*,#6899,.F.);
#9672=ORIENTED_EDGE('',*,*,#6896,.F.);
#9673=ORIENTED_EDGE('',*,*,#6900,.T.);
#9674=ORIENTED_EDGE('',*,*,#6886,.T.);
#9675=ORIENTED_EDGE('',*,*,#6900,.F.);
#9676=ORIENTED_EDGE('',*,*,#6895,.F.);
#9677=ORIENTED_EDGE('',*,*,#6901,.T.);
#9678=ORIENTED_EDGE('',*,*,#6887,.T.);
#9679=ORIENTED_EDGE('',*,*,#6901,.F.);
#9680=ORIENTED_EDGE('',*,*,#6898,.F.);
#9681=ORIENTED_EDGE('',*,*,#6902,.T.);
#9682=ORIENTED_EDGE('',*,*,#6888,.T.);
#9683=ORIENTED_EDGE('',*,*,#6902,.F.);
#9684=ORIENTED_EDGE('',*,*,#6897,.F.);
#9685=ORIENTED_EDGE('',*,*,#6899,.T.);
#9686=ORIENTED_EDGE('',*,*,#6884,.F.);
#9687=ORIENTED_EDGE('',*,*,#6870,.F.);
#9688=ORIENTED_EDGE('',*,*,#6890,.F.);
#9689=ORIENTED_EDGE('',*,*,#6878,.F.);
#9690=ORIENTED_EDGE('',*,*,#6881,.F.);
#9691=ORIENTED_EDGE('',*,*,#6844,.F.);
#9692=ORIENTED_EDGE('',*,*,#6893,.F.);
#9693=ORIENTED_EDGE('',*,*,#6854,.F.);
#9694=ORIENTED_EDGE('',*,*,#6825,.F.);
#9695=ORIENTED_EDGE('',*,*,#6861,.F.);
#9696=ORIENTED_EDGE('',*,*,#6867,.F.);
#9697=ORIENTED_EDGE('',*,*,#6883,.F.);
#9698=ORIENTED_EDGE('',*,*,#6858,.F.);
#9699=ORIENTED_EDGE('',*,*,#6891,.F.);
#9700=ORIENTED_EDGE('',*,*,#6868,.F.);
#9701=ORIENTED_EDGE('',*,*,#6865,.F.);
#9702=ORIENTED_EDGE('',*,*,#6834,.F.);
#9703=ORIENTED_EDGE('',*,*,#6894,.F.);
#9704=ORIENTED_EDGE('',*,*,#6842,.F.);
#9705=ORIENTED_EDGE('',*,*,#6839,.F.);
#9706=ORIENTED_EDGE('',*,*,#6830,.F.);
#9707=ORIENTED_EDGE('',*,*,#6841,.F.);
#9708=ORIENTED_EDGE('',*,*,#6846,.F.);
#9709=ORIENTED_EDGE('',*,*,#6880,.F.);
#9710=ORIENTED_EDGE('',*,*,#6828,.F.);
#9711=ORIENTED_EDGE('',*,*,#6903,.T.);
#9712=ORIENTED_EDGE('',*,*,#6875,.F.);
#9713=ORIENTED_EDGE('',*,*,#6904,.T.);
#9714=ORIENTED_EDGE('',*,*,#6905,.T.);
#9715=ORIENTED_EDGE('',*,*,#6836,.T.);
#9716=ORIENTED_EDGE('',*,*,#6906,.F.);
#9717=ORIENTED_EDGE('',*,*,#6907,.T.);
#9718=ORIENTED_EDGE('',*,*,#6873,.F.);
#9719=ORIENTED_EDGE('',*,*,#6908,.T.);
#9720=ORIENTED_EDGE('',*,*,#6831,.T.);
#9721=ORIENTED_EDGE('',*,*,#6838,.F.);
#9722=ORIENTED_EDGE('',*,*,#6905,.F.);
#9723=ORIENTED_EDGE('',*,*,#6909,.T.);
#9724=ORIENTED_EDGE('',*,*,#6906,.T.);
#9725=ORIENTED_EDGE('',*,*,#6837,.T.);
#9726=ORIENTED_EDGE('',*,*,#6817,.T.);
#9727=ORIENTED_EDGE('',*,*,#6823,.T.);
#9728=ORIENTED_EDGE('',*,*,#6910,.T.);
#9729=ORIENTED_EDGE('',*,*,#6851,.F.);
#9730=ORIENTED_EDGE('',*,*,#6911,.T.);
#9731=ORIENTED_EDGE('',*,*,#6912,.F.);
#9732=ORIENTED_EDGE('',*,*,#6862,.T.);
#9733=ORIENTED_EDGE('',*,*,#6913,.T.);
#9734=ORIENTED_EDGE('',*,*,#6914,.T.);
#9735=ORIENTED_EDGE('',*,*,#6849,.F.);
#9736=ORIENTED_EDGE('',*,*,#6915,.T.);
#9737=ORIENTED_EDGE('',*,*,#6855,.F.);
#9738=ORIENTED_EDGE('',*,*,#6864,.F.);
#9739=ORIENTED_EDGE('',*,*,#6912,.T.);
#9740=ORIENTED_EDGE('',*,*,#6916,.T.);
#9741=ORIENTED_EDGE('',*,*,#6913,.F.);
#9742=ORIENTED_EDGE('',*,*,#6863,.T.);
#9743=ORIENTED_EDGE('',*,*,#6818,.T.);
#9744=ORIENTED_EDGE('',*,*,#6889,.F.);
#9745=ORIENTED_EDGE('',*,*,#6832,.F.);
#9746=ORIENTED_EDGE('',*,*,#6908,.F.);
#9747=ORIENTED_EDGE('',*,*,#6872,.F.);
#9748=ORIENTED_EDGE('',*,*,#6907,.F.);
#9749=ORIENTED_EDGE('',*,*,#6909,.F.);
#9750=ORIENTED_EDGE('',*,*,#6904,.F.);
#9751=ORIENTED_EDGE('',*,*,#6874,.F.);
#9752=ORIENTED_EDGE('',*,*,#6903,.F.);
#9753=ORIENTED_EDGE('',*,*,#6827,.F.);
#9754=ORIENTED_EDGE('',*,*,#6879,.F.);
#9755=ORIENTED_EDGE('',*,*,#6876,.F.);
#9756=ORIENTED_EDGE('',*,*,#6915,.F.);
#9757=ORIENTED_EDGE('',*,*,#6848,.F.);
#9758=ORIENTED_EDGE('',*,*,#6892,.F.);
#9759=ORIENTED_EDGE('',*,*,#6856,.F.);
#9760=ORIENTED_EDGE('',*,*,#6914,.F.);
#9761=ORIENTED_EDGE('',*,*,#6916,.F.);
#9762=ORIENTED_EDGE('',*,*,#6911,.F.);
#9763=ORIENTED_EDGE('',*,*,#6850,.F.);
#9764=ORIENTED_EDGE('',*,*,#6882,.F.);
#9765=ORIENTED_EDGE('',*,*,#6852,.F.);
#9766=ORIENTED_EDGE('',*,*,#6910,.F.);
#9767=ORIENTED_EDGE('',*,*,#6822,.F.);
#9768=ORIENTED_EDGE('',*,*,#6917,.F.);
#9769=ORIENTED_EDGE('',*,*,#6918,.T.);
#9770=ORIENTED_EDGE('',*,*,#6919,.T.);
#9771=ORIENTED_EDGE('',*,*,#6918,.F.);
#9772=ORIENTED_EDGE('',*,*,#6920,.F.);
#9773=ORIENTED_EDGE('',*,*,#6921,.T.);
#9774=ORIENTED_EDGE('',*,*,#6922,.T.);
#9775=ORIENTED_EDGE('',*,*,#6921,.F.);
#9776=ORIENTED_EDGE('',*,*,#6923,.F.);
#9777=ORIENTED_EDGE('',*,*,#6924,.T.);
#9778=ORIENTED_EDGE('',*,*,#6925,.F.);
#9779=ORIENTED_EDGE('',*,*,#6926,.T.);
#9780=ORIENTED_EDGE('',*,*,#6927,.F.);
#9781=ORIENTED_EDGE('',*,*,#6928,.F.);
#9782=ORIENTED_EDGE('',*,*,#6929,.F.);
#9783=ORIENTED_EDGE('',*,*,#6930,.F.);
#9784=ORIENTED_EDGE('',*,*,#6931,.F.);
#9785=ORIENTED_EDGE('',*,*,#6932,.F.);
#9786=ORIENTED_EDGE('',*,*,#6933,.F.);
#9787=ORIENTED_EDGE('',*,*,#6934,.T.);
#9788=ORIENTED_EDGE('',*,*,#6935,.F.);
#9789=ORIENTED_EDGE('',*,*,#6936,.F.);
#9790=ORIENTED_EDGE('',*,*,#6937,.F.);
#9791=ORIENTED_EDGE('',*,*,#6938,.F.);
#9792=ORIENTED_EDGE('',*,*,#6939,.T.);
#9793=ORIENTED_EDGE('',*,*,#6935,.T.);
#9794=ORIENTED_EDGE('',*,*,#6940,.F.);
#9795=ORIENTED_EDGE('',*,*,#6931,.T.);
#9796=ORIENTED_EDGE('',*,*,#6941,.F.);
#9797=ORIENTED_EDGE('',*,*,#6942,.F.);
#9798=ORIENTED_EDGE('',*,*,#6943,.F.);
#9799=ORIENTED_EDGE('',*,*,#6944,.T.);
#9800=ORIENTED_EDGE('',*,*,#6923,.T.);
#9801=ORIENTED_EDGE('',*,*,#6945,.F.);
#9802=ORIENTED_EDGE('',*,*,#6946,.F.);
#9803=ORIENTED_EDGE('',*,*,#6947,.T.);
#9804=ORIENTED_EDGE('',*,*,#6936,.T.);
#9805=ORIENTED_EDGE('',*,*,#6939,.F.);
#9806=ORIENTED_EDGE('',*,*,#6927,.T.);
#9807=ORIENTED_EDGE('',*,*,#6948,.T.);
#9808=ORIENTED_EDGE('',*,*,#6949,.F.);
#9809=ORIENTED_EDGE('',*,*,#6941,.T.);
#9810=ORIENTED_EDGE('',*,*,#6930,.T.);
#9811=ORIENTED_EDGE('',*,*,#6950,.F.);
#9812=ORIENTED_EDGE('',*,*,#6951,.F.);
#9813=ORIENTED_EDGE('',*,*,#6952,.T.);
#9814=ORIENTED_EDGE('',*,*,#6925,.T.);
#9815=ORIENTED_EDGE('',*,*,#6953,.T.);
#9816=ORIENTED_EDGE('',*,*,#6954,.F.);
#9817=ORIENTED_EDGE('',*,*,#6955,.T.);
#9818=ORIENTED_EDGE('',*,*,#6954,.T.);
#9819=ORIENTED_EDGE('',*,*,#6956,.T.);
#9820=ORIENTED_EDGE('',*,*,#6943,.T.);
#9821=ORIENTED_EDGE('',*,*,#6938,.T.);
#9822=ORIENTED_EDGE('',*,*,#6957,.F.);
#9823=ORIENTED_EDGE('',*,*,#6958,.F.);
#9824=ORIENTED_EDGE('',*,*,#6959,.T.);
#9825=ORIENTED_EDGE('',*,*,#6942,.T.);
#9826=ORIENTED_EDGE('',*,*,#6949,.T.);
#9827=ORIENTED_EDGE('',*,*,#6960,.T.);
#9828=ORIENTED_EDGE('',*,*,#6919,.F.);
#9829=ORIENTED_EDGE('',*,*,#6937,.T.);
#9830=ORIENTED_EDGE('',*,*,#6934,.F.);
#9831=ORIENTED_EDGE('',*,*,#6961,.F.);
#9832=ORIENTED_EDGE('',*,*,#6957,.T.);
#9833=ORIENTED_EDGE('',*,*,#6940,.T.);
#9834=ORIENTED_EDGE('',*,*,#6959,.F.);
#9835=ORIENTED_EDGE('',*,*,#6962,.F.);
#9836=ORIENTED_EDGE('',*,*,#6932,.T.);
#9837=ORIENTED_EDGE('',*,*,#6961,.T.);
#9838=ORIENTED_EDGE('',*,*,#6933,.T.);
#9839=ORIENTED_EDGE('',*,*,#6962,.T.);
#9840=ORIENTED_EDGE('',*,*,#6958,.T.);
#9841=ORIENTED_EDGE('',*,*,#6929,.T.);
#9842=ORIENTED_EDGE('',*,*,#6947,.F.);
#9843=ORIENTED_EDGE('',*,*,#6963,.F.);
#9844=ORIENTED_EDGE('',*,*,#6950,.T.);
#9845=ORIENTED_EDGE('',*,*,#6928,.T.);
#9846=ORIENTED_EDGE('',*,*,#6952,.F.);
#9847=ORIENTED_EDGE('',*,*,#6964,.F.);
#9848=ORIENTED_EDGE('',*,*,#6945,.T.);
#9849=ORIENTED_EDGE('',*,*,#6951,.T.);
#9850=ORIENTED_EDGE('',*,*,#6963,.T.);
#9851=ORIENTED_EDGE('',*,*,#6946,.T.);
#9852=ORIENTED_EDGE('',*,*,#6964,.T.);
#9853=ORIENTED_EDGE('',*,*,#6920,.T.);
#9854=ORIENTED_EDGE('',*,*,#6956,.F.);
#9855=ORIENTED_EDGE('',*,*,#6953,.F.);
#9856=ORIENTED_EDGE('',*,*,#6924,.F.);
#9857=ORIENTED_EDGE('',*,*,#6944,.F.);
#9858=ORIENTED_EDGE('',*,*,#6960,.F.);
#9859=ORIENTED_EDGE('',*,*,#6948,.F.);
#9860=ORIENTED_EDGE('',*,*,#6926,.F.);
#9861=ORIENTED_EDGE('',*,*,#6955,.F.);
#9862=ORIENTED_EDGE('',*,*,#6917,.T.);
#9863=ORIENTED_EDGE('',*,*,#6922,.F.);
#9864=ORIENTED_EDGE('',*,*,#6965,.T.);
#9865=ORIENTED_EDGE('',*,*,#6966,.T.);
#9866=ORIENTED_EDGE('',*,*,#6967,.T.);
#9867=ORIENTED_EDGE('',*,*,#6968,.T.);
#9868=ORIENTED_EDGE('',*,*,#6969,.T.);
#9869=ORIENTED_EDGE('',*,*,#6970,.T.);
#9870=ORIENTED_EDGE('',*,*,#6971,.T.);
#9871=ORIENTED_EDGE('',*,*,#6972,.T.);
#9872=ORIENTED_EDGE('',*,*,#6973,.F.);
#9873=ORIENTED_EDGE('',*,*,#6974,.F.);
#9874=ORIENTED_EDGE('',*,*,#6975,.F.);
#9875=ORIENTED_EDGE('',*,*,#6976,.F.);
#9876=ORIENTED_EDGE('',*,*,#6977,.F.);
#9877=ORIENTED_EDGE('',*,*,#6978,.T.);
#9878=ORIENTED_EDGE('',*,*,#6979,.F.);
#9879=ORIENTED_EDGE('',*,*,#6980,.T.);
#9880=ORIENTED_EDGE('',*,*,#6981,.F.);
#9881=ORIENTED_EDGE('',*,*,#6982,.T.);
#9882=ORIENTED_EDGE('',*,*,#6983,.F.);
#9883=ORIENTED_EDGE('',*,*,#6984,.T.);
#9884=ORIENTED_EDGE('',*,*,#6985,.T.);
#9885=ORIENTED_EDGE('',*,*,#6986,.T.);
#9886=ORIENTED_EDGE('',*,*,#6987,.T.);
#9887=ORIENTED_EDGE('',*,*,#6988,.T.);
#9888=ORIENTED_EDGE('',*,*,#6967,.F.);
#9889=ORIENTED_EDGE('',*,*,#6989,.T.);
#9890=ORIENTED_EDGE('',*,*,#6977,.T.);
#9891=ORIENTED_EDGE('',*,*,#6990,.T.);
#9892=ORIENTED_EDGE('',*,*,#6969,.F.);
#9893=ORIENTED_EDGE('',*,*,#6991,.T.);
#9894=ORIENTED_EDGE('',*,*,#6983,.T.);
#9895=ORIENTED_EDGE('',*,*,#6992,.T.);
#9896=ORIENTED_EDGE('',*,*,#6981,.T.);
#9897=ORIENTED_EDGE('',*,*,#6993,.T.);
#9898=ORIENTED_EDGE('',*,*,#6971,.F.);
#9899=ORIENTED_EDGE('',*,*,#6994,.T.);
#9900=ORIENTED_EDGE('',*,*,#6979,.T.);
#9901=ORIENTED_EDGE('',*,*,#6995,.T.);
#9902=ORIENTED_EDGE('',*,*,#6965,.F.);
#9903=ORIENTED_EDGE('',*,*,#6996,.T.);
#9904=ORIENTED_EDGE('',*,*,#6985,.F.);
#9905=ORIENTED_EDGE('',*,*,#6997,.F.);
#9906=ORIENTED_EDGE('',*,*,#6974,.T.);
#9907=ORIENTED_EDGE('',*,*,#6998,.T.);
#9908=ORIENTED_EDGE('',*,*,#6986,.F.);
#9909=ORIENTED_EDGE('',*,*,#6998,.F.);
#9910=ORIENTED_EDGE('',*,*,#6973,.T.);
#9911=ORIENTED_EDGE('',*,*,#6999,.T.);
#9912=ORIENTED_EDGE('',*,*,#6987,.F.);
#9913=ORIENTED_EDGE('',*,*,#6999,.F.);
#9914=ORIENTED_EDGE('',*,*,#6976,.T.);
#9915=ORIENTED_EDGE('',*,*,#7000,.T.);
#9916=ORIENTED_EDGE('',*,*,#6988,.F.);
#9917=ORIENTED_EDGE('',*,*,#7000,.F.);
#9918=ORIENTED_EDGE('',*,*,#6975,.T.);
#9919=ORIENTED_EDGE('',*,*,#6997,.T.);
#9920=ORIENTED_EDGE('',*,*,#6966,.F.);
#9921=ORIENTED_EDGE('',*,*,#6995,.F.);
#9922=ORIENTED_EDGE('',*,*,#6978,.F.);
#9923=ORIENTED_EDGE('',*,*,#6989,.F.);
#9924=ORIENTED_EDGE('',*,*,#6972,.F.);
#9925=ORIENTED_EDGE('',*,*,#6993,.F.);
#9926=ORIENTED_EDGE('',*,*,#6980,.F.);
#9927=ORIENTED_EDGE('',*,*,#6996,.F.);
#9928=ORIENTED_EDGE('',*,*,#6968,.F.);
#9929=ORIENTED_EDGE('',*,*,#6990,.F.);
#9930=ORIENTED_EDGE('',*,*,#6984,.F.);
#9931=ORIENTED_EDGE('',*,*,#6991,.F.);
#9932=ORIENTED_EDGE('',*,*,#6970,.F.);
#9933=ORIENTED_EDGE('',*,*,#6992,.F.);
#9934=ORIENTED_EDGE('',*,*,#6982,.F.);
#9935=ORIENTED_EDGE('',*,*,#6994,.F.);
#9936=ORIENTED_EDGE('',*,*,#7001,.F.);
#9937=ORIENTED_EDGE('',*,*,#7002,.T.);
#9938=ORIENTED_EDGE('',*,*,#7003,.T.);
#9939=ORIENTED_EDGE('',*,*,#7002,.F.);
#9940=ORIENTED_EDGE('',*,*,#7004,.F.);
#9941=ORIENTED_EDGE('',*,*,#7005,.F.);
#9942=ORIENTED_EDGE('',*,*,#7006,.T.);
#9943=ORIENTED_EDGE('',*,*,#7007,.T.);
#9944=ORIENTED_EDGE('',*,*,#7006,.F.);
#9945=ORIENTED_EDGE('',*,*,#7004,.T.);
#9946=ORIENTED_EDGE('',*,*,#7005,.T.);
#9947=ORIENTED_EDGE('',*,*,#7008,.T.);
#9948=ORIENTED_EDGE('',*,*,#7009,.F.);
#9949=ORIENTED_EDGE('',*,*,#7008,.F.);
#9950=ORIENTED_EDGE('',*,*,#7010,.F.);
#9951=ORIENTED_EDGE('',*,*,#7011,.T.);
#9952=ORIENTED_EDGE('',*,*,#7012,.T.);
#9953=ORIENTED_EDGE('',*,*,#7011,.F.);
#9954=ORIENTED_EDGE('',*,*,#7013,.T.);
#9955=ORIENTED_EDGE('',*,*,#7014,.T.);
#9956=ORIENTED_EDGE('',*,*,#7015,.F.);
#9957=ORIENTED_EDGE('',*,*,#7014,.F.);
#9958=ORIENTED_EDGE('',*,*,#7016,.T.);
#9959=ORIENTED_EDGE('',*,*,#7017,.T.);
#9960=ORIENTED_EDGE('',*,*,#7018,.F.);
#9961=ORIENTED_EDGE('',*,*,#7017,.F.);
#9962=ORIENTED_EDGE('',*,*,#7019,.T.);
#9963=ORIENTED_EDGE('',*,*,#7020,.T.);
#9964=ORIENTED_EDGE('',*,*,#7021,.T.);
#9965=ORIENTED_EDGE('',*,*,#7020,.F.);
#9966=ORIENTED_EDGE('',*,*,#7007,.F.);
#9967=ORIENTED_EDGE('',*,*,#7010,.T.);
#9968=ORIENTED_EDGE('',*,*,#7009,.T.);
#9969=ORIENTED_EDGE('',*,*,#7013,.F.);
#9970=ORIENTED_EDGE('',*,*,#7015,.T.);
#9971=ORIENTED_EDGE('',*,*,#7019,.F.);
#9972=ORIENTED_EDGE('',*,*,#7012,.F.);
#9973=ORIENTED_EDGE('',*,*,#7018,.T.);
#9974=ORIENTED_EDGE('',*,*,#7003,.F.);
#9975=ORIENTED_EDGE('',*,*,#7021,.F.);
#9976=ORIENTED_EDGE('',*,*,#7001,.T.);
#9977=ORIENTED_EDGE('',*,*,#7016,.F.);
#9978=ORIENTED_EDGE('',*,*,#7022,.T.);
#9979=ORIENTED_EDGE('',*,*,#7022,.F.);
#9980=ORIENTED_EDGE('',*,*,#7023,.T.);
#9981=ORIENTED_EDGE('',*,*,#7023,.F.);
#9982=ORIENTED_EDGE('',*,*,#7024,.T.);
#9983=ORIENTED_EDGE('',*,*,#7024,.F.);
#9984=ORIENTED_EDGE('',*,*,#7025,.T.);
#9985=ORIENTED_EDGE('',*,*,#7025,.F.);
#9986=ORIENTED_EDGE('',*,*,#7026,.T.);
#9987=ORIENTED_EDGE('',*,*,#7026,.F.);
#9988=ORIENTED_EDGE('',*,*,#7027,.T.);
#9989=ORIENTED_EDGE('',*,*,#7027,.F.);
#9990=ORIENTED_EDGE('',*,*,#7028,.T.);
#9991=ORIENTED_EDGE('',*,*,#7028,.F.);
#9992=ORIENTED_EDGE('',*,*,#7029,.F.);
#9993=ORIENTED_EDGE('',*,*,#7030,.T.);
#9994=ORIENTED_EDGE('',*,*,#7031,.T.);
#9995=ORIENTED_EDGE('',*,*,#7030,.F.);
#9996=ORIENTED_EDGE('',*,*,#7032,.F.);
#9997=ORIENTED_EDGE('',*,*,#7033,.T.);
#9998=ORIENTED_EDGE('',*,*,#7029,.T.);
#9999=ORIENTED_EDGE('',*,*,#7033,.F.);
#10000=ORIENTED_EDGE('',*,*,#7034,.F.);
#10001=ORIENTED_EDGE('',*,*,#7035,.T.);
#10002=ORIENTED_EDGE('',*,*,#7032,.T.);
#10003=ORIENTED_EDGE('',*,*,#7035,.F.);
#10004=ORIENTED_EDGE('',*,*,#7036,.F.);
#10005=ORIENTED_EDGE('',*,*,#7037,.T.);
#10006=ORIENTED_EDGE('',*,*,#7038,.T.);
#10007=ORIENTED_EDGE('',*,*,#7037,.F.);
#10008=ORIENTED_EDGE('',*,*,#7039,.F.);
#10009=ORIENTED_EDGE('',*,*,#7040,.T.);
#10010=ORIENTED_EDGE('',*,*,#7036,.T.);
#10011=ORIENTED_EDGE('',*,*,#7040,.F.);
#10012=ORIENTED_EDGE('',*,*,#7041,.F.);
#10013=ORIENTED_EDGE('',*,*,#7042,.T.);
#10014=ORIENTED_EDGE('',*,*,#7039,.T.);
#10015=ORIENTED_EDGE('',*,*,#7042,.F.);
#10016=ORIENTED_EDGE('',*,*,#7043,.F.);
#10017=ORIENTED_EDGE('',*,*,#7044,.T.);
#10018=ORIENTED_EDGE('',*,*,#7041,.T.);
#10019=ORIENTED_EDGE('',*,*,#7044,.F.);
#10020=ORIENTED_EDGE('',*,*,#7045,.F.);
#10021=ORIENTED_EDGE('',*,*,#7046,.T.);
#10022=ORIENTED_EDGE('',*,*,#7043,.T.);
#10023=ORIENTED_EDGE('',*,*,#7046,.F.);
#10024=ORIENTED_EDGE('',*,*,#7047,.F.);
#10025=ORIENTED_EDGE('',*,*,#7048,.F.);
#10026=ORIENTED_EDGE('',*,*,#7049,.T.);
#10027=ORIENTED_EDGE('',*,*,#7045,.T.);
#10028=ORIENTED_EDGE('',*,*,#7049,.F.);
#10029=ORIENTED_EDGE('',*,*,#7047,.T.);
#10030=ORIENTED_EDGE('',*,*,#7048,.T.);
#10031=ORIENTED_EDGE('',*,*,#7050,.T.);
#10032=ORIENTED_EDGE('',*,*,#7051,.F.);
#10033=ORIENTED_EDGE('',*,*,#7052,.F.);
#10034=ORIENTED_EDGE('',*,*,#7050,.F.);
#10035=ORIENTED_EDGE('',*,*,#7053,.F.);
#10036=ORIENTED_EDGE('',*,*,#7054,.T.);
#10037=ORIENTED_EDGE('',*,*,#7051,.T.);
#10038=ORIENTED_EDGE('',*,*,#7052,.T.);
#10039=ORIENTED_EDGE('',*,*,#7054,.F.);
#10040=ORIENTED_EDGE('',*,*,#7055,.F.);
#10041=ORIENTED_EDGE('',*,*,#7056,.T.);
#10042=ORIENTED_EDGE('',*,*,#7053,.T.);
#10043=ORIENTED_EDGE('',*,*,#7056,.F.);
#10044=ORIENTED_EDGE('',*,*,#7031,.F.);
#10045=ORIENTED_EDGE('',*,*,#7055,.T.);
#10046=ORIENTED_EDGE('',*,*,#7034,.T.);
#10047=ORIENTED_EDGE('',*,*,#7038,.F.);
#10048=ORIENTED_EDGE('',*,*,#7057,.F.);
#10049=ORIENTED_EDGE('',*,*,#7058,.T.);
#10050=ORIENTED_EDGE('',*,*,#7059,.T.);
#10051=ORIENTED_EDGE('',*,*,#7058,.F.);
#10052=ORIENTED_EDGE('',*,*,#7060,.F.);
#10053=ORIENTED_EDGE('',*,*,#7061,.T.);
#10054=ORIENTED_EDGE('',*,*,#7062,.T.);
#10055=ORIENTED_EDGE('',*,*,#7061,.F.);
#10056=ORIENTED_EDGE('',*,*,#7063,.F.);
#10057=ORIENTED_EDGE('',*,*,#7064,.T.);
#10058=ORIENTED_EDGE('',*,*,#7060,.T.);
#10059=ORIENTED_EDGE('',*,*,#7064,.F.);
#10060=ORIENTED_EDGE('',*,*,#7065,.F.);
#10061=ORIENTED_EDGE('',*,*,#7066,.F.);
#10062=ORIENTED_EDGE('',*,*,#7067,.T.);
#10063=ORIENTED_EDGE('',*,*,#7063,.T.);
#10064=ORIENTED_EDGE('',*,*,#7067,.F.);
#10065=ORIENTED_EDGE('',*,*,#7065,.T.);
#10066=ORIENTED_EDGE('',*,*,#7066,.T.);
#10067=ORIENTED_EDGE('',*,*,#7068,.T.);
#10068=ORIENTED_EDGE('',*,*,#7069,.F.);
#10069=ORIENTED_EDGE('',*,*,#7068,.F.);
#10070=ORIENTED_EDGE('',*,*,#7070,.T.);
#10071=ORIENTED_EDGE('',*,*,#7071,.T.);
#10072=ORIENTED_EDGE('',*,*,#7072,.F.);
#10073=ORIENTED_EDGE('',*,*,#7071,.F.);
#10074=ORIENTED_EDGE('',*,*,#7073,.T.);
#10075=ORIENTED_EDGE('',*,*,#7074,.T.);
#10076=ORIENTED_EDGE('',*,*,#7075,.T.);
#10077=ORIENTED_EDGE('',*,*,#7076,.F.);
#10078=ORIENTED_EDGE('',*,*,#7075,.F.);
#10079=ORIENTED_EDGE('',*,*,#7077,.T.);
#10080=ORIENTED_EDGE('',*,*,#7078,.F.);
#10081=ORIENTED_EDGE('',*,*,#7079,.T.);
#10082=ORIENTED_EDGE('',*,*,#7080,.T.);
#10083=ORIENTED_EDGE('',*,*,#7079,.F.);
#10084=ORIENTED_EDGE('',*,*,#7081,.F.);
#10085=ORIENTED_EDGE('',*,*,#7082,.F.);
#10086=ORIENTED_EDGE('',*,*,#7083,.T.);
#10087=ORIENTED_EDGE('',*,*,#7084,.T.);
#10088=ORIENTED_EDGE('',*,*,#7083,.F.);
#10089=ORIENTED_EDGE('',*,*,#7081,.T.);
#10090=ORIENTED_EDGE('',*,*,#7082,.T.);
#10091=ORIENTED_EDGE('',*,*,#7085,.T.);
#10092=ORIENTED_EDGE('',*,*,#7086,.F.);
#10093=ORIENTED_EDGE('',*,*,#7087,.F.);
#10094=ORIENTED_EDGE('',*,*,#7085,.F.);
#10095=ORIENTED_EDGE('',*,*,#7074,.F.);
#10096=ORIENTED_EDGE('',*,*,#7088,.T.);
#10097=ORIENTED_EDGE('',*,*,#7086,.T.);
#10098=ORIENTED_EDGE('',*,*,#7087,.T.);
#10099=ORIENTED_EDGE('',*,*,#7088,.F.);
#10100=ORIENTED_EDGE('',*,*,#7077,.F.);
#10101=ORIENTED_EDGE('',*,*,#7059,.F.);
#10102=ORIENTED_EDGE('',*,*,#7089,.T.);
#10103=ORIENTED_EDGE('',*,*,#7078,.T.);
#10104=ORIENTED_EDGE('',*,*,#7089,.F.);
#10105=ORIENTED_EDGE('',*,*,#7090,.F.);
#10106=ORIENTED_EDGE('',*,*,#7091,.T.);
#10107=ORIENTED_EDGE('',*,*,#7092,.T.);
#10108=ORIENTED_EDGE('',*,*,#7091,.F.);
#10109=ORIENTED_EDGE('',*,*,#7093,.F.);
#10110=ORIENTED_EDGE('',*,*,#7094,.T.);
#10111=ORIENTED_EDGE('',*,*,#7090,.T.);
#10112=ORIENTED_EDGE('',*,*,#7094,.F.);
#10113=ORIENTED_EDGE('',*,*,#7095,.F.);
#10114=ORIENTED_EDGE('',*,*,#7096,.T.);
#10115=ORIENTED_EDGE('',*,*,#7097,.T.);
#10116=ORIENTED_EDGE('',*,*,#7096,.F.);
#10117=ORIENTED_EDGE('',*,*,#7098,.F.);
#10118=ORIENTED_EDGE('',*,*,#7099,.T.);
#10119=ORIENTED_EDGE('',*,*,#7095,.T.);
#10120=ORIENTED_EDGE('',*,*,#7099,.F.);
#10121=ORIENTED_EDGE('',*,*,#7100,.F.);
#10122=ORIENTED_EDGE('',*,*,#7101,.T.);
#10123=ORIENTED_EDGE('',*,*,#7098,.T.);
#10124=ORIENTED_EDGE('',*,*,#7101,.F.);
#10125=ORIENTED_EDGE('',*,*,#7102,.F.);
#10126=ORIENTED_EDGE('',*,*,#7103,.T.);
#10127=ORIENTED_EDGE('',*,*,#7104,.T.);
#10128=ORIENTED_EDGE('',*,*,#7103,.F.);
#10129=ORIENTED_EDGE('',*,*,#7105,.F.);
#10130=ORIENTED_EDGE('',*,*,#7106,.T.);
#10131=ORIENTED_EDGE('',*,*,#7102,.T.);
#10132=ORIENTED_EDGE('',*,*,#7106,.F.);
#10133=ORIENTED_EDGE('',*,*,#7070,.F.);
#10134=ORIENTED_EDGE('',*,*,#7107,.T.);
#10135=ORIENTED_EDGE('',*,*,#7057,.T.);
#10136=ORIENTED_EDGE('',*,*,#7107,.F.);
#10137=ORIENTED_EDGE('',*,*,#7073,.F.);
#10138=ORIENTED_EDGE('',*,*,#7104,.F.);
#10139=ORIENTED_EDGE('',*,*,#7100,.T.);
#10140=ORIENTED_EDGE('',*,*,#7093,.T.);
#10141=ORIENTED_EDGE('',*,*,#7097,.F.);
#10142=ORIENTED_EDGE('',*,*,#7084,.F.);
#10143=ORIENTED_EDGE('',*,*,#7105,.T.);
#10144=ORIENTED_EDGE('',*,*,#7076,.T.);
#10145=ORIENTED_EDGE('',*,*,#7080,.F.);
#10146=ORIENTED_EDGE('',*,*,#7062,.F.);
#10147=ORIENTED_EDGE('',*,*,#7072,.T.);
#10148=ORIENTED_EDGE('',*,*,#7069,.T.);
#10149=ORIENTED_EDGE('',*,*,#7092,.F.);
#10150=CYLINDRICAL_SURFACE('',#11161,2.);
#10151=CYLINDRICAL_SURFACE('',#11164,2.);
#10152=CYLINDRICAL_SURFACE('',#11167,4.);
#10153=CYLINDRICAL_SURFACE('',#11170,2.25);
#10154=CYLINDRICAL_SURFACE('',#11173,4.);
#10155=CYLINDRICAL_SURFACE('',#11176,2.25);
#10156=CYLINDRICAL_SURFACE('',#11179,7.00000000000001);
#10157=CYLINDRICAL_SURFACE('',#11182,10.);
#10158=CYLINDRICAL_SURFACE('',#11185,11.1);
#10159=CYLINDRICAL_SURFACE('',#11196,12.5);
#10160=CYLINDRICAL_SURFACE('',#11209,2.);
#10161=CYLINDRICAL_SURFACE('',#11210,2.);
#10162=CYLINDRICAL_SURFACE('',#11234,2.);
#10163=CYLINDRICAL_SURFACE('',#11237,2.);
#10164=CYLINDRICAL_SURFACE('',#11240,4.);
#10165=CYLINDRICAL_SURFACE('',#11243,2.25);
#10166=CYLINDRICAL_SURFACE('',#11246,4.);
#10167=CYLINDRICAL_SURFACE('',#11249,2.25);
#10168=CYLINDRICAL_SURFACE('',#11252,7.00000000000001);
#10169=CYLINDRICAL_SURFACE('',#11255,10.);
#10170=CYLINDRICAL_SURFACE('',#11258,11.1);
#10171=CYLINDRICAL_SURFACE('',#11269,12.5);
#10172=CYLINDRICAL_SURFACE('',#11282,2.);
#10173=CYLINDRICAL_SURFACE('',#11283,2.);
#10174=CYLINDRICAL_SURFACE('',#11307,4.);
#10175=CYLINDRICAL_SURFACE('',#11312,2.25);
#10176=CYLINDRICAL_SURFACE('',#11315,4.);
#10177=CYLINDRICAL_SURFACE('',#11318,2.25);
#10178=CYLINDRICAL_SURFACE('',#11321,7.00000000000001);
#10179=CYLINDRICAL_SURFACE('',#11324,10.);
#10180=CYLINDRICAL_SURFACE('',#11327,11.1);
#10181=CYLINDRICAL_SURFACE('',#11336,12.5);
#10182=CYLINDRICAL_SURFACE('',#11350,2.);
#10183=CYLINDRICAL_SURFACE('',#11351,2.);
#10184=CYLINDRICAL_SURFACE('',#11360,4.);
#10185=CYLINDRICAL_SURFACE('',#11361,4.);
#10186=CYLINDRICAL_SURFACE('',#11367,4.);
#10187=CYLINDRICAL_SURFACE('',#11372,2.25);
#10188=CYLINDRICAL_SURFACE('',#11375,4.);
#10189=CYLINDRICAL_SURFACE('',#11378,2.25);
#10190=CYLINDRICAL_SURFACE('',#11381,7.00000000000001);
#10191=CYLINDRICAL_SURFACE('',#11384,10.);
#10192=CYLINDRICAL_SURFACE('',#11387,11.1);
#10193=CYLINDRICAL_SURFACE('',#11396,12.5);
#10194=CYLINDRICAL_SURFACE('',#11410,2.);
#10195=CYLINDRICAL_SURFACE('',#11411,2.);
#10196=CYLINDRICAL_SURFACE('',#11420,4.);
#10197=CYLINDRICAL_SURFACE('',#11421,4.);
#10198=CYLINDRICAL_SURFACE('',#11427,3.);
#10199=CYLINDRICAL_SURFACE('',#11430,3.);
#10200=CYLINDRICAL_SURFACE('',#11433,3.25);
#10201=CYLINDRICAL_SURFACE('',#11436,3.25);
#10202=CYLINDRICAL_SURFACE('',#11439,2.25);
#10203=CYLINDRICAL_SURFACE('',#11442,1.75);
#10204=CYLINDRICAL_SURFACE('',#11445,1.75);
#10205=CYLINDRICAL_SURFACE('',#11448,3.);
#10206=CYLINDRICAL_SURFACE('',#11451,1.5);
#10207=CYLINDRICAL_SURFACE('',#11454,1.5);
#10208=CYLINDRICAL_SURFACE('',#11460,4.);
#10209=CYLINDRICAL_SURFACE('',#11463,4.);
#10210=CYLINDRICAL_SURFACE('',#11467,3.);
#10211=CYLINDRICAL_SURFACE('',#11471,3.);
#10212=CYLINDRICAL_SURFACE('',#11475,3.);
#10213=CYLINDRICAL_SURFACE('',#11479,3.);
#10214=CYLINDRICAL_SURFACE('',#11487,5.);
#10215=CYLINDRICAL_SURFACE('',#11490,5.);
#10216=CYLINDRICAL_SURFACE('',#11493,5.);
#10217=CYLINDRICAL_SURFACE('',#11496,5.);
#10218=CYLINDRICAL_SURFACE('',#11499,5.);
#10219=CYLINDRICAL_SURFACE('',#11502,5.);
#10220=CYLINDRICAL_SURFACE('',#11530,7.);
#10221=CYLINDRICAL_SURFACE('',#11531,5.);
#10222=CYLINDRICAL_SURFACE('',#11534,7.);
#10223=CYLINDRICAL_SURFACE('',#11544,2.7);
#10224=CYLINDRICAL_SURFACE('',#11546,2.7);
#10225=CYLINDRICAL_SURFACE('',#11548,4.);
#10226=CYLINDRICAL_SURFACE('',#11569,12.);
#10227=CYLINDRICAL_SURFACE('',#11570,10.);
#10228=CYLINDRICAL_SURFACE('',#11573,12.);
#10229=CYLINDRICAL_SURFACE('',#11584,2.);
#10230=CYLINDRICAL_SURFACE('',#11586,1.);
#10231=CYLINDRICAL_SURFACE('',#11589,1.);
#10232=CYLINDRICAL_SURFACE('',#11592,1.5);
#10233=CYLINDRICAL_SURFACE('',#11595,1.5);
#10234=CYLINDRICAL_SURFACE('',#11598,1.);
#10235=CYLINDRICAL_SURFACE('',#11601,2.75);
#10236=CYLINDRICAL_SURFACE('',#11611,10.2500000000004);
#10237=CYLINDRICAL_SURFACE('',#11614,11.25);
#10238=CYLINDRICAL_SURFACE('',#11618,2.75);
#10239=CYLINDRICAL_SURFACE('',#11633,11.25);
#10240=CYLINDRICAL_SURFACE('',#11640,3.);
#10241=CYLINDRICAL_SURFACE('',#11642,3.);
#10242=CYLINDRICAL_SURFACE('',#11647,10.2500000000004);
#10243=CYLINDRICAL_SURFACE('',#11652,1.5);
#10244=CYLINDRICAL_SURFACE('',#11654,1.5);
#10245=CYLINDRICAL_SURFACE('',#11671,5.);
#10246=CYLINDRICAL_SURFACE('',#11674,6.);
#10247=CYLINDRICAL_SURFACE('',#11684,11.);
#10248=CYLINDRICAL_SURFACE('',#11687,10.);
#10249=CYLINDRICAL_SURFACE('',#11690,12.7);
#10250=CYLINDRICAL_SURFACE('',#11693,14.7);
#10251=CYLINDRICAL_SURFACE('',#11705,14.7);
#10252=CYLINDRICAL_SURFACE('',#11710,12.7);
#10253=CYLINDRICAL_SURFACE('',#11713,3.65);
#10254=CYLINDRICAL_SURFACE('',#11857,0.200000403400263);
#10255=CYLINDRICAL_SURFACE('',#11859,0.600000196920858);
#10256=CYLINDRICAL_SURFACE('',#11861,0.200000373597978);
#10257=CYLINDRICAL_SURFACE('',#11863,0.199999419924102);
#10258=CYLINDRICAL_SURFACE('',#11865,0.20000038104856);
#10259=CYLINDRICAL_SURFACE('',#11867,1.99999965375783);
#10260=CYLINDRICAL_SURFACE('',#11869,0.200000284191204);
#10261=CYLINDRICAL_SURFACE('',#11871,0.200000284191204);
#10262=CYLINDRICAL_SURFACE('',#11873,0.200000284191218);
#10263=CYLINDRICAL_SURFACE('',#11875,0.60000037573478);
#10264=CYLINDRICAL_SURFACE('',#11877,0.200000284191204);
#10265=CYLINDRICAL_SURFACE('',#11886,0.20000028419119);
#10266=CYLINDRICAL_SURFACE('',#11888,0.60000037573478);
#10267=CYLINDRICAL_SURFACE('',#11890,0.200000284191218);
#10268=CYLINDRICAL_SURFACE('',#11892,0.200000284191204);
#10269=CYLINDRICAL_SURFACE('',#11894,0.200000284191218);
#10270=CYLINDRICAL_SURFACE('',#11896,1.99999965375781);
#10271=CYLINDRICAL_SURFACE('',#11898,0.200000381048546);
#10272=CYLINDRICAL_SURFACE('',#11900,0.199999419924102);
#10273=CYLINDRICAL_SURFACE('',#11902,0.200000373597978);
#10274=CYLINDRICAL_SURFACE('',#11904,0.600000196920858);
#10275=CYLINDRICAL_SURFACE('',#11906,0.200000403400263);
#10276=CYLINDRICAL_SURFACE('',#11915,0.200000403400263);
#10277=CYLINDRICAL_SURFACE('',#11917,0.600000196920858);
#10278=CYLINDRICAL_SURFACE('',#11919,0.200000373597978);
#10279=CYLINDRICAL_SURFACE('',#11921,0.199999419924102);
#10280=CYLINDRICAL_SURFACE('',#11923,0.200000381048546);
#10281=CYLINDRICAL_SURFACE('',#11925,1.99999965375781);
#10282=CYLINDRICAL_SURFACE('',#11927,0.200000284191204);
#10283=CYLINDRICAL_SURFACE('',#11929,0.200000284191204);
#10284=CYLINDRICAL_SURFACE('',#11931,0.200000284191218);
#10285=CYLINDRICAL_SURFACE('',#11933,0.600000375734794);
#10286=CYLINDRICAL_SURFACE('',#11935,0.200000284191204);
#10287=CYLINDRICAL_SURFACE('',#11944,0.200000284191204);
#10288=CYLINDRICAL_SURFACE('',#11946,0.60000037573478);
#10289=CYLINDRICAL_SURFACE('',#11948,0.200000284191218);
#10290=CYLINDRICAL_SURFACE('',#11950,0.20000028419119);
#10291=CYLINDRICAL_SURFACE('',#11952,0.200000284191218);
#10292=CYLINDRICAL_SURFACE('',#11954,1.9999996537578);
#10293=CYLINDRICAL_SURFACE('',#11956,0.200000381048532);
#10294=CYLINDRICAL_SURFACE('',#11958,0.199999419924102);
#10295=CYLINDRICAL_SURFACE('',#11960,0.200000373597992);
#10296=CYLINDRICAL_SURFACE('',#11962,0.600000196920844);
#10297=CYLINDRICAL_SURFACE('',#11964,0.200000403400263);
#10298=CYLINDRICAL_SURFACE('',#11968,0.999999990441758);
#10299=CYLINDRICAL_SURFACE('',#11970,0.999999990441772);
#10300=CYLINDRICAL_SURFACE('',#11972,0.999999990441772);
#10301=CYLINDRICAL_SURFACE('',#11974,0.999999990441758);
#10302=CYLINDRICAL_SURFACE('',#11976,3.65);
#10303=CYLINDRICAL_SURFACE('',#11978,5.50000000000001);
#10304=CYLINDRICAL_SURFACE('',#11981,5.50000000000001);
#10305=CYLINDRICAL_SURFACE('',#11983,3.65);
#10306=CYLINDRICAL_SURFACE('',#11985,5.50000000000001);
#10307=CYLINDRICAL_SURFACE('',#11987,3.65);
#10308=CYLINDRICAL_SURFACE('',#11989,5.50000000000001);
#10309=CYLINDRICAL_SURFACE('',#11991,0.999999990441758);
#10310=CYLINDRICAL_SURFACE('',#11993,0.999999990441758);
#10311=CYLINDRICAL_SURFACE('',#11995,0.999999990441758);
#10312=CYLINDRICAL_SURFACE('',#11997,0.999999990441758);
#10313=CYLINDRICAL_SURFACE('',#11999,0.999999990441758);
#10314=CYLINDRICAL_SURFACE('',#12001,0.999999990441758);
#10315=CYLINDRICAL_SURFACE('',#12003,0.999999990441772);
#10316=CYLINDRICAL_SURFACE('',#12005,0.999999990441772);
#10317=CYLINDRICAL_SURFACE('',#12007,0.999999990441758);
#10318=CYLINDRICAL_SURFACE('',#12009,0.999999990441758);
#10319=CYLINDRICAL_SURFACE('',#12011,0.999999990441758);
#10320=CYLINDRICAL_SURFACE('',#12013,0.999999990441758);
#10321=CYLINDRICAL_SURFACE('',#12016,2.25);
#10322=CYLINDRICAL_SURFACE('',#12019,2.25);
#10323=CYLINDRICAL_SURFACE('',#12054,4.);
#10324=CYLINDRICAL_SURFACE('',#12056,4.);
#10325=CYLINDRICAL_SURFACE('',#12058,2.);
#10326=CYLINDRICAL_SURFACE('',#12059,2.);
#10327=CYLINDRICAL_SURFACE('',#12060,5.);
#10328=CYLINDRICAL_SURFACE('',#12061,5.);
#10329=CYLINDRICAL_SURFACE('',#12062,5.);
#10330=CYLINDRICAL_SURFACE('',#12063,5.);
#10331=CYLINDRICAL_SURFACE('',#12078,2.);
#10332=CYLINDRICAL_SURFACE('',#12079,2.);
#10333=CYLINDRICAL_SURFACE('',#12080,2.);
#10334=CYLINDRICAL_SURFACE('',#12081,2.);
#10335=CYLINDRICAL_SURFACE('',#12082,2.);
#10336=CYLINDRICAL_SURFACE('',#12083,2.);
#10337=CYLINDRICAL_SURFACE('',#12085,3.99999999999999);
#10338=CYLINDRICAL_SURFACE('',#12088,2.15);
#10339=CYLINDRICAL_SURFACE('',#12109,4.);
#10340=CYLINDRICAL_SURFACE('',#12110,4.);
#10341=CYLINDRICAL_SURFACE('',#12131,4.);
#10342=CYLINDRICAL_SURFACE('',#12132,4.);
#10343=CYLINDRICAL_SURFACE('',#12133,4.);
#10344=CYLINDRICAL_SURFACE('',#12134,4.);
#10345=CYLINDRICAL_SURFACE('',#12136,9.);
#10346=CYLINDRICAL_SURFACE('',#12145,6.2);
#10347=CYLINDRICAL_SURFACE('',#12148,6.2);
#10348=CYLINDRICAL_SURFACE('',#12151,4.2);
#10349=CYLINDRICAL_SURFACE('',#12154,4.2);
#10350=CYLINDRICAL_SURFACE('',#12182,11.);
#10351=CYLINDRICAL_SURFACE('',#12187,9.6);
#10352=CYLINDRICAL_SURFACE('',#12195,8.8);
#10353=CYLINDRICAL_SURFACE('',#12200,8.8);
#10354=CYLINDRICAL_SURFACE('',#12209,9.6);
#10355=CYLINDRICAL_SURFACE('',#12220,9.6);
#10356=CYLINDRICAL_SURFACE('',#12245,9.6);
#10357=CYLINDRICAL_SURFACE('',#12246,6.075);
#10358=CYLINDRICAL_SURFACE('',#12247,6.075);
#10359=CYLINDRICAL_SURFACE('',#12257,4.);
#10360=CYLINDRICAL_SURFACE('',#12266,6.075);
#10361=CYLINDRICAL_SURFACE('',#12268,6.075);
#10362=ADVANCED_FACE('',(#725),#10150,.F.);
#10363=ADVANCED_FACE('',(#726),#10151,.F.);
#10364=ADVANCED_FACE('',(#727),#10152,.F.);
#10365=ADVANCED_FACE('',(#728),#10153,.F.);
#10366=ADVANCED_FACE('',(#729),#10154,.F.);
#10367=ADVANCED_FACE('',(#730),#10155,.F.);
#10368=ADVANCED_FACE('',(#731),#10156,.F.);
#10369=ADVANCED_FACE('',(#732),#10157,.F.);
#10370=ADVANCED_FACE('',(#733),#10158,.F.);
#10371=ADVANCED_FACE('',(#734),#381,.F.);
#10372=ADVANCED_FACE('',(#735),#382,.F.);
#10373=ADVANCED_FACE('',(#736),#383,.F.);
#10374=ADVANCED_FACE('',(#737,#251,#252,#253),#384,.F.);
#10375=ADVANCED_FACE('',(#738),#385,.T.);
#10376=ADVANCED_FACE('',(#739),#10159,.T.);
#10377=ADVANCED_FACE('',(#740),#386,.T.);
#10378=ADVANCED_FACE('',(#741),#387,.F.);
#10379=ADVANCED_FACE('',(#742),#388,.F.);
#10380=ADVANCED_FACE('',(#743,#254,#255,#256,#257,#258),#389,.T.);
#10381=ADVANCED_FACE('',(#744,#259),#390,.T.);
#10382=ADVANCED_FACE('',(#745,#260),#391,.T.);
#10383=ADVANCED_FACE('',(#746),#392,.F.);
#10384=ADVANCED_FACE('',(#747),#393,.F.);
#10385=ADVANCED_FACE('',(#748),#394,.T.);
#10386=ADVANCED_FACE('',(#749),#10160,.T.);
#10387=ADVANCED_FACE('',(#750),#10161,.T.);
#10388=ADVANCED_FACE('',(#751,#261),#395,.F.);
#10389=ADVANCED_FACE('',(#752,#262),#396,.F.);
#10390=ADVANCED_FACE('',(#753),#397,.F.);
#10391=ADVANCED_FACE('',(#754),#398,.F.);
#10392=ADVANCED_FACE('',(#755),#399,.F.);
#10393=ADVANCED_FACE('',(#756),#400,.F.);
#10394=ADVANCED_FACE('',(#757),#401,.F.);
#10395=ADVANCED_FACE('',(#758),#402,.F.);
#10396=ADVANCED_FACE('',(#759,#263),#403,.F.);
#10397=ADVANCED_FACE('',(#760),#404,.F.);
#10398=ADVANCED_FACE('',(#761),#405,.F.);
#10399=ADVANCED_FACE('',(#762),#406,.F.);
#10400=ADVANCED_FACE('',(#763),#407,.F.);
#10401=ADVANCED_FACE('',(#764),#408,.F.);
#10402=ADVANCED_FACE('',(#765),#409,.F.);
#10403=ADVANCED_FACE('',(#766,#264),#410,.T.);
#10404=ADVANCED_FACE('',(#767),#411,.T.);
#10405=ADVANCED_FACE('',(#768),#412,.T.);
#10406=ADVANCED_FACE('',(#769),#413,.F.);
#10407=ADVANCED_FACE('',(#770,#265,#266),#414,.T.);
#10408=ADVANCED_FACE('',(#771),#415,.F.);
#10409=ADVANCED_FACE('',(#772),#416,.F.);
#10410=ADVANCED_FACE('',(#773),#10162,.F.);
#10411=ADVANCED_FACE('',(#774),#10163,.F.);
#10412=ADVANCED_FACE('',(#775),#10164,.F.);
#10413=ADVANCED_FACE('',(#776),#10165,.F.);
#10414=ADVANCED_FACE('',(#777),#10166,.F.);
#10415=ADVANCED_FACE('',(#778),#10167,.F.);
#10416=ADVANCED_FACE('',(#779),#10168,.F.);
#10417=ADVANCED_FACE('',(#780),#10169,.F.);
#10418=ADVANCED_FACE('',(#781),#10170,.F.);
#10419=ADVANCED_FACE('',(#782),#417,.F.);
#10420=ADVANCED_FACE('',(#783),#418,.F.);
#10421=ADVANCED_FACE('',(#784),#419,.F.);
#10422=ADVANCED_FACE('',(#785,#267,#268,#269),#420,.F.);
#10423=ADVANCED_FACE('',(#786),#421,.T.);
#10424=ADVANCED_FACE('',(#787),#10171,.T.);
#10425=ADVANCED_FACE('',(#788),#422,.T.);
#10426=ADVANCED_FACE('',(#789),#423,.F.);
#10427=ADVANCED_FACE('',(#790),#424,.F.);
#10428=ADVANCED_FACE('',(#791,#270,#271,#272,#273,#274),#425,.T.);
#10429=ADVANCED_FACE('',(#792,#275),#426,.T.);
#10430=ADVANCED_FACE('',(#793,#276),#427,.T.);
#10431=ADVANCED_FACE('',(#794),#428,.F.);
#10432=ADVANCED_FACE('',(#795),#429,.F.);
#10433=ADVANCED_FACE('',(#796),#430,.T.);
#10434=ADVANCED_FACE('',(#797),#10172,.T.);
#10435=ADVANCED_FACE('',(#798),#10173,.T.);
#10436=ADVANCED_FACE('',(#799,#277),#431,.F.);
#10437=ADVANCED_FACE('',(#800,#278),#432,.F.);
#10438=ADVANCED_FACE('',(#801),#433,.F.);
#10439=ADVANCED_FACE('',(#802),#434,.F.);
#10440=ADVANCED_FACE('',(#803),#435,.F.);
#10441=ADVANCED_FACE('',(#804),#436,.F.);
#10442=ADVANCED_FACE('',(#805),#437,.F.);
#10443=ADVANCED_FACE('',(#806),#438,.F.);
#10444=ADVANCED_FACE('',(#807,#279),#439,.F.);
#10445=ADVANCED_FACE('',(#808),#440,.F.);
#10446=ADVANCED_FACE('',(#809),#441,.F.);
#10447=ADVANCED_FACE('',(#810),#442,.F.);
#10448=ADVANCED_FACE('',(#811),#443,.F.);
#10449=ADVANCED_FACE('',(#812),#444,.F.);
#10450=ADVANCED_FACE('',(#813),#445,.F.);
#10451=ADVANCED_FACE('',(#814,#280),#446,.T.);
#10452=ADVANCED_FACE('',(#815),#447,.T.);
#10453=ADVANCED_FACE('',(#816),#448,.T.);
#10454=ADVANCED_FACE('',(#817),#449,.F.);
#10455=ADVANCED_FACE('',(#818,#281,#282),#450,.T.);
#10456=ADVANCED_FACE('',(#819),#451,.F.);
#10457=ADVANCED_FACE('',(#820),#452,.F.);
#10458=ADVANCED_FACE('',(#821),#10174,.F.);
#10459=ADVANCED_FACE('',(#822),#10175,.F.);
#10460=ADVANCED_FACE('',(#823),#10176,.F.);
#10461=ADVANCED_FACE('',(#824),#10177,.F.);
#10462=ADVANCED_FACE('',(#825),#10178,.F.);
#10463=ADVANCED_FACE('',(#826),#10179,.F.);
#10464=ADVANCED_FACE('',(#827),#10180,.F.);
#10465=ADVANCED_FACE('',(#828),#453,.F.);
#10466=ADVANCED_FACE('',(#829),#454,.F.);
#10467=ADVANCED_FACE('',(#830),#455,.F.);
#10468=ADVANCED_FACE('',(#831),#456,.T.);
#10469=ADVANCED_FACE('',(#832),#10181,.T.);
#10470=ADVANCED_FACE('',(#833),#457,.T.);
#10471=ADVANCED_FACE('',(#834),#458,.F.);
#10472=ADVANCED_FACE('',(#835),#459,.F.);
#10473=ADVANCED_FACE('',(#836,#283,#284),#460,.T.);
#10474=ADVANCED_FACE('',(#837,#285),#461,.F.);
#10475=ADVANCED_FACE('',(#838,#286),#462,.T.);
#10476=ADVANCED_FACE('',(#839,#287),#463,.T.);
#10477=ADVANCED_FACE('',(#840),#10182,.T.);
#10478=ADVANCED_FACE('',(#841),#10183,.T.);
#10479=ADVANCED_FACE('',(#842,#288),#464,.F.);
#10480=ADVANCED_FACE('',(#843,#289),#465,.F.);
#10481=ADVANCED_FACE('',(#844),#466,.F.);
#10482=ADVANCED_FACE('',(#845),#467,.F.);
#10483=ADVANCED_FACE('',(#846),#468,.F.);
#10484=ADVANCED_FACE('',(#847),#469,.T.);
#10485=ADVANCED_FACE('',(#848),#10184,.T.);
#10486=ADVANCED_FACE('',(#849),#10185,.T.);
#10487=ADVANCED_FACE('',(#850),#470,.F.);
#10488=ADVANCED_FACE('',(#851,#290,#291),#471,.F.);
#10489=ADVANCED_FACE('',(#852),#472,.F.);
#10490=ADVANCED_FACE('',(#853),#473,.F.);
#10491=ADVANCED_FACE('',(#854),#10186,.F.);
#10492=ADVANCED_FACE('',(#855),#10187,.F.);
#10493=ADVANCED_FACE('',(#856),#10188,.F.);
#10494=ADVANCED_FACE('',(#857),#10189,.F.);
#10495=ADVANCED_FACE('',(#858),#10190,.F.);
#10496=ADVANCED_FACE('',(#859),#10191,.F.);
#10497=ADVANCED_FACE('',(#860),#10192,.F.);
#10498=ADVANCED_FACE('',(#861),#474,.F.);
#10499=ADVANCED_FACE('',(#862),#475,.F.);
#10500=ADVANCED_FACE('',(#863),#476,.F.);
#10501=ADVANCED_FACE('',(#864),#477,.T.);
#10502=ADVANCED_FACE('',(#865),#10193,.T.);
#10503=ADVANCED_FACE('',(#866),#478,.T.);
#10504=ADVANCED_FACE('',(#867),#479,.F.);
#10505=ADVANCED_FACE('',(#868),#480,.F.);
#10506=ADVANCED_FACE('',(#869,#292,#293),#481,.T.);
#10507=ADVANCED_FACE('',(#870,#294),#482,.F.);
#10508=ADVANCED_FACE('',(#871,#295),#483,.T.);
#10509=ADVANCED_FACE('',(#872,#296),#484,.T.);
#10510=ADVANCED_FACE('',(#873),#10194,.T.);
#10511=ADVANCED_FACE('',(#874),#10195,.T.);
#10512=ADVANCED_FACE('',(#875,#297),#485,.F.);
#10513=ADVANCED_FACE('',(#876,#298),#486,.F.);
#10514=ADVANCED_FACE('',(#877),#487,.F.);
#10515=ADVANCED_FACE('',(#878),#488,.F.);
#10516=ADVANCED_FACE('',(#879),#489,.F.);
#10517=ADVANCED_FACE('',(#880),#490,.T.);
#10518=ADVANCED_FACE('',(#881),#10196,.T.);
#10519=ADVANCED_FACE('',(#882),#10197,.T.);
#10520=ADVANCED_FACE('',(#883),#491,.F.);
#10521=ADVANCED_FACE('',(#884,#299,#300),#492,.F.);
#10522=ADVANCED_FACE('',(#885),#493,.F.);
#10523=ADVANCED_FACE('',(#886),#494,.F.);
#10524=ADVANCED_FACE('',(#887),#10198,.F.);
#10525=ADVANCED_FACE('',(#888),#10199,.F.);
#10526=ADVANCED_FACE('',(#889),#10200,.F.);
#10527=ADVANCED_FACE('',(#890),#10201,.F.);
#10528=ADVANCED_FACE('',(#891),#10202,.F.);
#10529=ADVANCED_FACE('',(#892),#10203,.F.);
#10530=ADVANCED_FACE('',(#893),#10204,.F.);
#10531=ADVANCED_FACE('',(#894),#10205,.F.);
#10532=ADVANCED_FACE('',(#895),#10206,.F.);
#10533=ADVANCED_FACE('',(#896),#10207,.F.);
#10534=ADVANCED_FACE('',(#897),#495,.F.);
#10535=ADVANCED_FACE('',(#898),#496,.F.);
#10536=ADVANCED_FACE('',(#899),#497,.F.);
#10537=ADVANCED_FACE('',(#900),#10208,.T.);
#10538=ADVANCED_FACE('',(#901),#10209,.T.);
#10539=ADVANCED_FACE('',(#902),#498,.T.);
#10540=ADVANCED_FACE('',(#903),#10210,.F.);
#10541=ADVANCED_FACE('',(#904),#499,.T.);
#10542=ADVANCED_FACE('',(#905),#10211,.F.);
#10543=ADVANCED_FACE('',(#906),#500,.F.);
#10544=ADVANCED_FACE('',(#907),#10212,.F.);
#10545=ADVANCED_FACE('',(#908),#501,.F.);
#10546=ADVANCED_FACE('',(#909),#10213,.F.);
#10547=ADVANCED_FACE('',(#910),#502,.T.);
#10548=ADVANCED_FACE('',(#911),#503,.T.);
#10549=ADVANCED_FACE('',(#912),#504,.T.);
#10550=ADVANCED_FACE('',(#913),#505,.T.);
#10551=ADVANCED_FACE('',(#914),#506,.T.);
#10552=ADVANCED_FACE('',(#915),#10214,.T.);
#10553=ADVANCED_FACE('',(#916),#10215,.F.);
#10554=ADVANCED_FACE('',(#917),#10216,.T.);
#10555=ADVANCED_FACE('',(#918),#10217,.T.);
#10556=ADVANCED_FACE('',(#919),#10218,.T.);
#10557=ADVANCED_FACE('',(#920),#10219,.F.);
#10558=ADVANCED_FACE('',(#921,#301,#302,#303,#304,#305,#306,#307),#507,
 .T.);
#10559=ADVANCED_FACE('',(#922,#308),#508,.F.);
#10560=ADVANCED_FACE('',(#923,#309),#509,.F.);
#10561=ADVANCED_FACE('',(#924,#310,#311,#312,#313,#314,#315,#316),#510,
 .T.);
#10562=ADVANCED_FACE('',(#925,#317),#511,.F.);
#10563=ADVANCED_FACE('',(#926,#318),#512,.F.);
#10564=ADVANCED_FACE('',(#927),#146,.T.);
#10565=ADVANCED_FACE('',(#928),#147,.T.);
#10566=ADVANCED_FACE('',(#929),#148,.T.);
#10567=ADVANCED_FACE('',(#930),#149,.T.);
#10568=ADVANCED_FACE('',(#931),#10220,.T.);
#10569=ADVANCED_FACE('',(#932),#10221,.T.);
#10570=ADVANCED_FACE('',(#933),#10222,.T.);
#10571=ADVANCED_FACE('',(#934,#319),#513,.F.);
#10572=ADVANCED_FACE('',(#935,#320),#514,.F.);
#10573=ADVANCED_FACE('',(#936,#321),#515,.F.);
#10574=ADVANCED_FACE('',(#937,#322),#516,.F.);
#10575=ADVANCED_FACE('',(#938),#517,.F.);
#10576=ADVANCED_FACE('',(#939),#10223,.F.);
#10577=ADVANCED_FACE('',(#940),#518,.T.);
#10578=ADVANCED_FACE('',(#941),#10224,.F.);
#10579=ADVANCED_FACE('',(#942),#10225,.F.);
#10580=ADVANCED_FACE('',(#943),#150,.T.);
#10581=ADVANCED_FACE('',(#944),#151,.T.);
#10582=ADVANCED_FACE('',(#945),#152,.T.);
#10583=ADVANCED_FACE('',(#946),#153,.T.);
#10584=ADVANCED_FACE('',(#947),#10226,.T.);
#10585=ADVANCED_FACE('',(#948),#10227,.T.);
#10586=ADVANCED_FACE('',(#949),#10228,.T.);
#10587=ADVANCED_FACE('',(#950,#323),#519,.F.);
#10588=ADVANCED_FACE('',(#951,#324),#520,.F.);
#10589=ADVANCED_FACE('',(#952,#325),#521,.F.);
#10590=ADVANCED_FACE('',(#953,#326),#522,.F.);
#10591=ADVANCED_FACE('',(#954),#154,.T.);
#10592=ADVANCED_FACE('',(#955),#10229,.T.);
#10593=ADVANCED_FACE('',(#956),#10230,.F.);
#10594=ADVANCED_FACE('',(#957),#10231,.F.);
#10595=ADVANCED_FACE('',(#958),#10232,.F.);
#10596=ADVANCED_FACE('',(#959),#10233,.F.);
#10597=ADVANCED_FACE('',(#960),#10234,.F.);
#10598=ADVANCED_FACE('',(#961),#10235,.T.);
#10599=ADVANCED_FACE('',(#962),#155,.T.);
#10600=ADVANCED_FACE('',(#963),#10236,.T.);
#10601=ADVANCED_FACE('',(#964),#10237,.T.);
#10602=ADVANCED_FACE('',(#965),#10238,.T.);
#10603=ADVANCED_FACE('',(#966,#327,#328,#329,#330,#331,#332),#523,.F.);
#10604=ADVANCED_FACE('',(#967,#333),#524,.T.);
#10605=ADVANCED_FACE('',(#968),#525,.T.);
#10606=ADVANCED_FACE('',(#969,#334),#526,.T.);
#10607=ADVANCED_FACE('',(#970),#10239,.T.);
#10608=ADVANCED_FACE('',(#971),#527,.T.);
#10609=ADVANCED_FACE('',(#972),#528,.T.);
#10610=ADVANCED_FACE('',(#973),#529,.T.);
#10611=ADVANCED_FACE('',(#974),#530,.T.);
#10612=ADVANCED_FACE('',(#975),#10240,.T.);
#10613=ADVANCED_FACE('',(#976),#10241,.T.);
#10614=ADVANCED_FACE('',(#977),#531,.T.);
#10615=ADVANCED_FACE('',(#978,#335,#336,#337,#338,#339),#532,.T.);
#10616=ADVANCED_FACE('',(#979),#533,.F.);
#10617=ADVANCED_FACE('',(#980),#10242,.T.);
#10618=ADVANCED_FACE('',(#981),#534,.F.);
#10619=ADVANCED_FACE('',(#982),#535,.F.);
#10620=ADVANCED_FACE('',(#983),#536,.T.);
#10621=ADVANCED_FACE('',(#984),#10243,.T.);
#10622=ADVANCED_FACE('',(#985),#156,.T.);
#10623=ADVANCED_FACE('',(#986),#10244,.T.);
#10624=ADVANCED_FACE('',(#987),#537,.T.);
#10625=ADVANCED_FACE('',(#988),#538,.T.);
#10626=ADVANCED_FACE('',(#989),#539,.F.);
#10627=ADVANCED_FACE('',(#990),#540,.T.);
#10628=ADVANCED_FACE('',(#991),#541,.F.);
#10629=ADVANCED_FACE('',(#992),#542,.T.);
#10630=ADVANCED_FACE('',(#993),#543,.T.);
#10631=ADVANCED_FACE('',(#994),#544,.T.);
#10632=ADVANCED_FACE('',(#995),#545,.T.);
#10633=ADVANCED_FACE('',(#996,#340),#546,.F.);
#10634=ADVANCED_FACE('',(#997),#547,.F.);
#10635=ADVANCED_FACE('',(#998,#341),#548,.F.);
#10636=ADVANCED_FACE('',(#999),#549,.F.);
#10637=ADVANCED_FACE('',(#1000),#550,.T.);
#10638=ADVANCED_FACE('',(#1001),#551,.T.);
#10639=ADVANCED_FACE('',(#1002),#10245,.F.);
#10640=ADVANCED_FACE('',(#1003),#10246,.T.);
#10641=ADVANCED_FACE('',(#1004,#342),#552,.T.);
#10642=ADVANCED_FACE('',(#1005,#343),#553,.F.);
#10643=ADVANCED_FACE('',(#1006),#554,.F.);
#10644=ADVANCED_FACE('',(#1007),#10247,.T.);
#10645=ADVANCED_FACE('',(#1008),#555,.F.);
#10646=ADVANCED_FACE('',(#1009),#556,.T.);
#10647=ADVANCED_FACE('',(#1010),#10248,.F.);
#10648=ADVANCED_FACE('',(#1011),#557,.T.);
#10649=ADVANCED_FACE('',(#1012),#10249,.F.);
#10650=ADVANCED_FACE('',(#1013),#10250,.T.);
#10651=ADVANCED_FACE('',(#1014,#344),#558,.T.);
#10652=ADVANCED_FACE('',(#1015,#345),#559,.F.);
#10653=ADVANCED_FACE('',(#1016),#560,.F.);
#10654=ADVANCED_FACE('',(#1017),#561,.F.);
#10655=ADVANCED_FACE('',(#1018),#562,.F.);
#10656=ADVANCED_FACE('',(#1019),#10251,.T.);
#10657=ADVANCED_FACE('',(#1020),#563,.F.);
#10658=ADVANCED_FACE('',(#1021),#564,.T.);
#10659=ADVANCED_FACE('',(#1022),#565,.T.);
#10660=ADVANCED_FACE('',(#1023),#566,.T.);
#10661=ADVANCED_FACE('',(#1024),#10252,.F.);
#10662=ADVANCED_FACE('',(#1025),#567,.T.);
#10663=ADVANCED_FACE('',(#1026),#10253,.F.);
#10664=ADVANCED_FACE('',(#1027,#346,#347,#348,#349,#350),#568,.T.);
#10665=ADVANCED_FACE('',(#1028,#351,#352,#353,#354,#355),#569,.F.);
#10666=ADVANCED_FACE('',(#1029),#570,.F.);
#10667=ADVANCED_FACE('',(#1030),#571,.F.);
#10668=ADVANCED_FACE('',(#1031),#572,.F.);
#10669=ADVANCED_FACE('',(#1032),#573,.F.);
#10670=ADVANCED_FACE('',(#1033),#574,.F.);
#10671=ADVANCED_FACE('',(#1034),#10254,.F.);
#10672=ADVANCED_FACE('',(#1035),#575,.F.);
#10673=ADVANCED_FACE('',(#1036),#10255,.T.);
#10674=ADVANCED_FACE('',(#1037),#576,.F.);
#10675=ADVANCED_FACE('',(#1038),#10256,.T.);
#10676=ADVANCED_FACE('',(#1039),#577,.F.);
#10677=ADVANCED_FACE('',(#1040),#10257,.F.);
#10678=ADVANCED_FACE('',(#1041),#578,.F.);
#10679=ADVANCED_FACE('',(#1042),#10258,.T.);
#10680=ADVANCED_FACE('',(#1043),#579,.F.);
#10681=ADVANCED_FACE('',(#1044),#10259,.T.);
#10682=ADVANCED_FACE('',(#1045),#580,.F.);
#10683=ADVANCED_FACE('',(#1046),#10260,.T.);
#10684=ADVANCED_FACE('',(#1047),#581,.F.);
#10685=ADVANCED_FACE('',(#1048),#10261,.F.);
#10686=ADVANCED_FACE('',(#1049),#582,.F.);
#10687=ADVANCED_FACE('',(#1050),#10262,.T.);
#10688=ADVANCED_FACE('',(#1051),#583,.F.);
#10689=ADVANCED_FACE('',(#1052),#10263,.T.);
#10690=ADVANCED_FACE('',(#1053),#584,.F.);
#10691=ADVANCED_FACE('',(#1054),#10264,.F.);
#10692=ADVANCED_FACE('',(#1055),#585,.F.);
#10693=ADVANCED_FACE('',(#1056),#586,.F.);
#10694=ADVANCED_FACE('',(#1057),#587,.F.);
#10695=ADVANCED_FACE('',(#1058),#588,.F.);
#10696=ADVANCED_FACE('',(#1059),#589,.F.);
#10697=ADVANCED_FACE('',(#1060),#590,.F.);
#10698=ADVANCED_FACE('',(#1061),#591,.F.);
#10699=ADVANCED_FACE('',(#1062),#592,.F.);
#10700=ADVANCED_FACE('',(#1063),#10265,.F.);
#10701=ADVANCED_FACE('',(#1064),#593,.F.);
#10702=ADVANCED_FACE('',(#1065),#10266,.T.);
#10703=ADVANCED_FACE('',(#1066),#594,.F.);
#10704=ADVANCED_FACE('',(#1067),#10267,.T.);
#10705=ADVANCED_FACE('',(#1068),#595,.F.);
#10706=ADVANCED_FACE('',(#1069),#10268,.F.);
#10707=ADVANCED_FACE('',(#1070),#596,.F.);
#10708=ADVANCED_FACE('',(#1071),#10269,.T.);
#10709=ADVANCED_FACE('',(#1072),#597,.F.);
#10710=ADVANCED_FACE('',(#1073),#10270,.T.);
#10711=ADVANCED_FACE('',(#1074),#598,.F.);
#10712=ADVANCED_FACE('',(#1075),#10271,.T.);
#10713=ADVANCED_FACE('',(#1076),#599,.F.);
#10714=ADVANCED_FACE('',(#1077),#10272,.F.);
#10715=ADVANCED_FACE('',(#1078),#600,.F.);
#10716=ADVANCED_FACE('',(#1079),#10273,.T.);
#10717=ADVANCED_FACE('',(#1080),#601,.F.);
#10718=ADVANCED_FACE('',(#1081),#10274,.T.);
#10719=ADVANCED_FACE('',(#1082),#602,.F.);
#10720=ADVANCED_FACE('',(#1083),#10275,.F.);
#10721=ADVANCED_FACE('',(#1084),#603,.F.);
#10722=ADVANCED_FACE('',(#1085),#604,.F.);
#10723=ADVANCED_FACE('',(#1086),#605,.F.);
#10724=ADVANCED_FACE('',(#1087),#606,.F.);
#10725=ADVANCED_FACE('',(#1088),#607,.F.);
#10726=ADVANCED_FACE('',(#1089),#608,.F.);
#10727=ADVANCED_FACE('',(#1090),#609,.F.);
#10728=ADVANCED_FACE('',(#1091),#610,.F.);
#10729=ADVANCED_FACE('',(#1092),#10276,.F.);
#10730=ADVANCED_FACE('',(#1093),#611,.F.);
#10731=ADVANCED_FACE('',(#1094),#10277,.T.);
#10732=ADVANCED_FACE('',(#1095),#612,.F.);
#10733=ADVANCED_FACE('',(#1096),#10278,.T.);
#10734=ADVANCED_FACE('',(#1097),#613,.F.);
#10735=ADVANCED_FACE('',(#1098),#10279,.F.);
#10736=ADVANCED_FACE('',(#1099),#614,.F.);
#10737=ADVANCED_FACE('',(#1100),#10280,.T.);
#10738=ADVANCED_FACE('',(#1101),#615,.F.);
#10739=ADVANCED_FACE('',(#1102),#10281,.T.);
#10740=ADVANCED_FACE('',(#1103),#616,.F.);
#10741=ADVANCED_FACE('',(#1104),#10282,.T.);
#10742=ADVANCED_FACE('',(#1105),#617,.F.);
#10743=ADVANCED_FACE('',(#1106),#10283,.F.);
#10744=ADVANCED_FACE('',(#1107),#618,.F.);
#10745=ADVANCED_FACE('',(#1108),#10284,.T.);
#10746=ADVANCED_FACE('',(#1109),#619,.F.);
#10747=ADVANCED_FACE('',(#1110),#10285,.T.);
#10748=ADVANCED_FACE('',(#1111),#620,.F.);
#10749=ADVANCED_FACE('',(#1112),#10286,.F.);
#10750=ADVANCED_FACE('',(#1113),#621,.F.);
#10751=ADVANCED_FACE('',(#1114),#622,.F.);
#10752=ADVANCED_FACE('',(#1115),#623,.F.);
#10753=ADVANCED_FACE('',(#1116),#624,.F.);
#10754=ADVANCED_FACE('',(#1117),#625,.F.);
#10755=ADVANCED_FACE('',(#1118),#626,.F.);
#10756=ADVANCED_FACE('',(#1119),#627,.F.);
#10757=ADVANCED_FACE('',(#1120),#628,.F.);
#10758=ADVANCED_FACE('',(#1121),#10287,.F.);
#10759=ADVANCED_FACE('',(#1122),#629,.F.);
#10760=ADVANCED_FACE('',(#1123),#10288,.T.);
#10761=ADVANCED_FACE('',(#1124),#630,.F.);
#10762=ADVANCED_FACE('',(#1125),#10289,.T.);
#10763=ADVANCED_FACE('',(#1126),#631,.F.);
#10764=ADVANCED_FACE('',(#1127),#10290,.F.);
#10765=ADVANCED_FACE('',(#1128),#632,.F.);
#10766=ADVANCED_FACE('',(#1129),#10291,.T.);
#10767=ADVANCED_FACE('',(#1130),#633,.F.);
#10768=ADVANCED_FACE('',(#1131),#10292,.T.);
#10769=ADVANCED_FACE('',(#1132),#634,.F.);
#10770=ADVANCED_FACE('',(#1133),#10293,.T.);
#10771=ADVANCED_FACE('',(#1134),#635,.F.);
#10772=ADVANCED_FACE('',(#1135),#10294,.F.);
#10773=ADVANCED_FACE('',(#1136),#636,.F.);
#10774=ADVANCED_FACE('',(#1137),#10295,.T.);
#10775=ADVANCED_FACE('',(#1138),#637,.F.);
#10776=ADVANCED_FACE('',(#1139),#10296,.T.);
#10777=ADVANCED_FACE('',(#1140),#638,.F.);
#10778=ADVANCED_FACE('',(#1141),#10297,.F.);
#10779=ADVANCED_FACE('',(#1142),#639,.F.);
#10780=ADVANCED_FACE('',(#1143),#640,.F.);
#10781=ADVANCED_FACE('',(#1144),#641,.F.);
#10782=ADVANCED_FACE('',(#1145),#10298,.F.);
#10783=ADVANCED_FACE('',(#1146),#642,.T.);
#10784=ADVANCED_FACE('',(#1147),#10299,.F.);
#10785=ADVANCED_FACE('',(#1148),#643,.T.);
#10786=ADVANCED_FACE('',(#1149),#10300,.F.);
#10787=ADVANCED_FACE('',(#1150),#644,.T.);
#10788=ADVANCED_FACE('',(#1151),#10301,.F.);
#10789=ADVANCED_FACE('',(#1152),#645,.T.);
#10790=ADVANCED_FACE('',(#1153),#10302,.F.);
#10791=ADVANCED_FACE('',(#1154),#646,.T.);
#10792=ADVANCED_FACE('',(#1155),#10303,.F.);
#10793=ADVANCED_FACE('',(#1156),#647,.T.);
#10794=ADVANCED_FACE('',(#1157),#648,.T.);
#10795=ADVANCED_FACE('',(#1158),#10304,.F.);
#10796=ADVANCED_FACE('',(#1159),#649,.T.);
#10797=ADVANCED_FACE('',(#1160),#10305,.F.);
#10798=ADVANCED_FACE('',(#1161),#650,.T.);
#10799=ADVANCED_FACE('',(#1162),#10306,.F.);
#10800=ADVANCED_FACE('',(#1163),#651,.T.);
#10801=ADVANCED_FACE('',(#1164),#10307,.F.);
#10802=ADVANCED_FACE('',(#1165),#652,.T.);
#10803=ADVANCED_FACE('',(#1166),#10308,.F.);
#10804=ADVANCED_FACE('',(#1167),#653,.T.);
#10805=ADVANCED_FACE('',(#1168),#10309,.F.);
#10806=ADVANCED_FACE('',(#1169),#654,.T.);
#10807=ADVANCED_FACE('',(#1170),#10310,.F.);
#10808=ADVANCED_FACE('',(#1171),#655,.T.);
#10809=ADVANCED_FACE('',(#1172),#10311,.F.);
#10810=ADVANCED_FACE('',(#1173),#656,.T.);
#10811=ADVANCED_FACE('',(#1174),#10312,.F.);
#10812=ADVANCED_FACE('',(#1175),#657,.T.);
#10813=ADVANCED_FACE('',(#1176),#10313,.F.);
#10814=ADVANCED_FACE('',(#1177),#658,.T.);
#10815=ADVANCED_FACE('',(#1178),#10314,.F.);
#10816=ADVANCED_FACE('',(#1179),#659,.T.);
#10817=ADVANCED_FACE('',(#1180),#10315,.F.);
#10818=ADVANCED_FACE('',(#1181),#660,.T.);
#10819=ADVANCED_FACE('',(#1182),#10316,.F.);
#10820=ADVANCED_FACE('',(#1183),#661,.T.);
#10821=ADVANCED_FACE('',(#1184),#10317,.F.);
#10822=ADVANCED_FACE('',(#1185),#662,.T.);
#10823=ADVANCED_FACE('',(#1186),#10318,.F.);
#10824=ADVANCED_FACE('',(#1187),#663,.T.);
#10825=ADVANCED_FACE('',(#1188),#10319,.F.);
#10826=ADVANCED_FACE('',(#1189),#664,.T.);
#10827=ADVANCED_FACE('',(#1190),#10320,.F.);
#10828=ADVANCED_FACE('',(#1191),#665,.T.);
#10829=ADVANCED_FACE('',(#1192),#10321,.F.);
#10830=ADVANCED_FACE('',(#1193),#10322,.F.);
#10831=ADVANCED_FACE('',(#1194),#666,.F.);
#10832=ADVANCED_FACE('',(#1195),#667,.T.);
#10833=ADVANCED_FACE('',(#1196),#668,.T.);
#10834=ADVANCED_FACE('',(#1197),#669,.F.);
#10835=ADVANCED_FACE('',(#1198,#356),#670,.T.);
#10836=ADVANCED_FACE('',(#1199),#671,.T.);
#10837=ADVANCED_FACE('',(#1200),#672,.F.);
#10838=ADVANCED_FACE('',(#1201),#673,.F.);
#10839=ADVANCED_FACE('',(#1202,#357),#674,.T.);
#10840=ADVANCED_FACE('',(#1203),#675,.F.);
#10841=ADVANCED_FACE('',(#1204,#358),#676,.T.);
#10842=ADVANCED_FACE('',(#1205,#359),#677,.F.);
#10843=ADVANCED_FACE('',(#1206),#10323,.F.);
#10844=ADVANCED_FACE('',(#1207),#678,.F.);
#10845=ADVANCED_FACE('',(#1208),#10324,.F.);
#10846=ADVANCED_FACE('',(#1209),#679,.F.);
#10847=ADVANCED_FACE('',(#1210),#10325,.F.);
#10848=ADVANCED_FACE('',(#1211),#10326,.F.);
#10849=ADVANCED_FACE('',(#1212),#10327,.T.);
#10850=ADVANCED_FACE('',(#1213),#10328,.T.);
#10851=ADVANCED_FACE('',(#1214),#10329,.T.);
#10852=ADVANCED_FACE('',(#1215),#10330,.T.);
#10853=ADVANCED_FACE('',(#1216),#680,.T.);
#10854=ADVANCED_FACE('',(#1217),#681,.F.);
#10855=ADVANCED_FACE('',(#1218,#360),#682,.T.);
#10856=ADVANCED_FACE('',(#1219),#683,.F.);
#10857=ADVANCED_FACE('',(#1220),#684,.T.);
#10858=ADVANCED_FACE('',(#1221,#361),#685,.T.);
#10859=ADVANCED_FACE('',(#1222),#10331,.T.);
#10860=ADVANCED_FACE('',(#1223),#10332,.T.);
#10861=ADVANCED_FACE('',(#1224),#10333,.T.);
#10862=ADVANCED_FACE('',(#1225),#10334,.T.);
#10863=ADVANCED_FACE('',(#1226),#10335,.T.);
#10864=ADVANCED_FACE('',(#1227),#10336,.T.);
#10865=ADVANCED_FACE('',(#1228),#10337,.F.);
#10866=ADVANCED_FACE('',(#1229),#10338,.F.);
#10867=ADVANCED_FACE('',(#1230),#686,.F.);
#10868=ADVANCED_FACE('',(#1231),#687,.F.);
#10869=ADVANCED_FACE('',(#1232),#688,.F.);
#10870=ADVANCED_FACE('',(#1233),#689,.F.);
#10871=ADVANCED_FACE('',(#1234),#690,.F.);
#10872=ADVANCED_FACE('',(#1235),#691,.F.);
#10873=ADVANCED_FACE('',(#1236),#692,.F.);
#10874=ADVANCED_FACE('',(#1237,#362),#693,.T.);
#10875=ADVANCED_FACE('',(#1238),#694,.F.);
#10876=ADVANCED_FACE('',(#1239),#695,.F.);
#10877=ADVANCED_FACE('',(#1240),#696,.T.);
#10878=ADVANCED_FACE('',(#1241),#697,.F.);
#10879=ADVANCED_FACE('',(#1242),#698,.F.);
#10880=ADVANCED_FACE('',(#1243,#363),#699,.T.);
#10881=ADVANCED_FACE('',(#1244),#10339,.T.);
#10882=ADVANCED_FACE('',(#1245),#10340,.T.);
#10883=ADVANCED_FACE('',(#1246,#364),#700,.F.);
#10884=ADVANCED_FACE('',(#1247,#365),#701,.T.);
#10885=ADVANCED_FACE('',(#1248,#366),#702,.F.);
#10886=ADVANCED_FACE('',(#1249),#703,.F.);
#10887=ADVANCED_FACE('',(#1250),#704,.F.);
#10888=ADVANCED_FACE('',(#1251),#705,.F.);
#10889=ADVANCED_FACE('',(#1252),#706,.F.);
#10890=ADVANCED_FACE('',(#1253),#707,.T.);
#10891=ADVANCED_FACE('',(#1254),#708,.T.);
#10892=ADVANCED_FACE('',(#1255),#709,.T.);
#10893=ADVANCED_FACE('',(#1256),#710,.T.);
#10894=ADVANCED_FACE('',(#1257),#10341,.T.);
#10895=ADVANCED_FACE('',(#1258),#10342,.T.);
#10896=ADVANCED_FACE('',(#1259),#10343,.T.);
#10897=ADVANCED_FACE('',(#1260),#10344,.T.);
#10898=ADVANCED_FACE('',(#1261),#10345,.F.);
#10899=ADVANCED_FACE('',(#1262),#130,.T.);
#10900=ADVANCED_FACE('',(#1263),#131,.T.);
#10901=ADVANCED_FACE('',(#1264),#10346,.T.);
#10902=ADVANCED_FACE('',(#1265),#10347,.T.);
#10903=ADVANCED_FACE('',(#1266),#10348,.F.);
#10904=ADVANCED_FACE('',(#1267),#10349,.F.);
#10905=ADVANCED_FACE('',(#1268,#367),#711,.F.);
#10906=ADVANCED_FACE('',(#1269,#368),#712,.T.);
#10907=ADVANCED_FACE('',(#1270,#369),#713,.T.);
#10908=ADVANCED_FACE('',(#1271,#370),#714,.T.);
#10909=ADVANCED_FACE('',(#1272,#371),#715,.T.);
#10910=ADVANCED_FACE('',(#1273,#372),#716,.T.);
#10911=ADVANCED_FACE('',(#1274),#123,.T.);
#10912=ADVANCED_FACE('',(#1275),#124,.T.);
#10913=ADVANCED_FACE('',(#1276),#125,.T.);
#10914=ADVANCED_FACE('',(#1277),#126,.T.);
#10915=ADVANCED_FACE('',(#1278),#127,.T.);
#10916=ADVANCED_FACE('',(#1279),#128,.T.);
#10917=ADVANCED_FACE('',(#1280),#129,.T.);
#10918=ADVANCED_FACE('',(#1281),#157,.T.);
#10919=ADVANCED_FACE('',(#1282),#10350,.T.);
#10920=ADVANCED_FACE('',(#1283),#158,.T.);
#10921=ADVANCED_FACE('',(#1284),#10351,.F.);
#10922=ADVANCED_FACE('',(#1285),#159,.F.);
#10923=ADVANCED_FACE('',(#1286),#132,.F.);
#10924=ADVANCED_FACE('',(#1287),#10352,.F.);
#10925=ADVANCED_FACE('',(#1288),#160,.F.);
#10926=ADVANCED_FACE('',(#1289),#10353,.F.);
#10927=ADVANCED_FACE('',(#1290),#133,.F.);
#10928=ADVANCED_FACE('',(#1291),#161,.F.);
#10929=ADVANCED_FACE('',(#1292),#10354,.F.);
#10930=ADVANCED_FACE('',(#1293,#373),#717,.T.);
#10931=ADVANCED_FACE('',(#1294,#374),#718,.T.);
#10932=ADVANCED_FACE('',(#1295),#162,.F.);
#10933=ADVANCED_FACE('',(#1296),#134,.T.);
#10934=ADVANCED_FACE('',(#1297),#10355,.T.);
#10935=ADVANCED_FACE('',(#1298),#135,.F.);
#10936=ADVANCED_FACE('',(#1299),#136,.T.);
#10937=ADVANCED_FACE('',(#1300),#137,.F.);
#10938=ADVANCED_FACE('',(#1301),#138,.T.);
#10939=ADVANCED_FACE('',(#1302),#139,.F.);
#10940=ADVANCED_FACE('',(#1303),#140,.T.);
#10941=ADVANCED_FACE('',(#1304),#141,.F.);
#10942=ADVANCED_FACE('',(#1305),#10356,.T.);
#10943=ADVANCED_FACE('',(#1306),#10357,.T.);
#10944=ADVANCED_FACE('',(#1307),#10358,.T.);
#10945=ADVANCED_FACE('',(#1308),#163,.T.);
#10946=ADVANCED_FACE('',(#1309),#164,.T.);
#10947=ADVANCED_FACE('',(#1310),#10359,.F.);
#10948=ADVANCED_FACE('',(#1311),#165,.T.);
#10949=ADVANCED_FACE('',(#1312),#166,.T.);
#10950=ADVANCED_FACE('',(#1313),#10360,.T.);
#10951=ADVANCED_FACE('',(#1314),#10361,.T.);
#10952=ADVANCED_FACE('',(#1315,#375),#719,.T.);
#10953=ADVANCED_FACE('',(#1316,#376),#720,.T.);
#10954=ADVANCED_FACE('',(#1317,#377),#721,.T.);
#10955=ADVANCED_FACE('',(#1318,#378),#722,.T.);
#10956=ADVANCED_FACE('',(#1319,#379),#723,.T.);
#10957=ADVANCED_FACE('',(#1320,#380),#724,.T.);
#10958=CLOSED_SHELL('',(#10362,#10363,#10364,#10365,#10366,#10367,#10368,
#10369,#10370,#10371,#10372,#10373,#10374,#10375,#10376,#10377,#10378,#10379,
#10380,#10381,#10382,#10383,#10384,#10385,#10386,#10387,#10388,#10389,#10390,
#10391,#10392,#10393,#10394,#10395,#10396,#10397,#10398,#10399,#10400,#10401,
#10402,#10403,#10404,#10405,#10406,#10407,#10408,#10409));
#10959=CLOSED_SHELL('',(#10410,#10411,#10412,#10413,#10414,#10415,#10416,
#10417,#10418,#10419,#10420,#10421,#10422,#10423,#10424,#10425,#10426,#10427,
#10428,#10429,#10430,#10431,#10432,#10433,#10434,#10435,#10436,#10437,#10438,
#10439,#10440,#10441,#10442,#10443,#10444,#10445,#10446,#10447,#10448,#10449,
#10450,#10451,#10452,#10453,#10454,#10455,#10456,#10457));
#10960=CLOSED_SHELL('',(#10458,#10459,#10460,#10461,#10462,#10463,#10464,
#10465,#10466,#10467,#10468,#10469,#10470,#10471,#10472,#10473,#10474,#10475,
#10476,#10477,#10478,#10479,#10480,#10481,#10482,#10483,#10484,#10485,#10486,
#10487,#10488,#10489,#10490));
#10961=CLOSED_SHELL('',(#10491,#10492,#10493,#10494,#10495,#10496,#10497,
#10498,#10499,#10500,#10501,#10502,#10503,#10504,#10505,#10506,#10507,#10508,
#10509,#10510,#10511,#10512,#10513,#10514,#10515,#10516,#10517,#10518,#10519,
#10520,#10521,#10522,#10523));
#10962=CLOSED_SHELL('',(#10524,#10525,#10526,#10527,#10528,#10529,#10530,
#10531,#10532,#10533,#10534,#10535,#10536,#10537,#10538,#10539,#10540,#10541,
#10542,#10543,#10544,#10545,#10546,#10547,#10548,#10549,#10550,#10551,#10552,
#10553,#10554,#10555,#10556,#10557,#10558,#10559,#10560,#10561,#10562,#10563));
#10963=CLOSED_SHELL('',(#10564,#10565,#10566,#10567,#10568,#10569,#10570,
#10571,#10572,#10573,#10574,#10575,#10576,#10577,#10578));
#10964=CLOSED_SHELL('',(#10579,#10580,#10581,#10582,#10583,#10584,#10585,
#10586,#10587,#10588,#10589,#10590));
#10965=CLOSED_SHELL('',(#10591,#10592,#10593,#10594,#10595,#10596,#10597,
#10598,#10599,#10600,#10601,#10602,#10603,#10604,#10605,#10606,#10607,#10608,
#10609,#10610,#10611,#10612,#10613,#10614,#10615,#10616,#10617,#10618,#10619,
#10620,#10621,#10622,#10623,#10624,#10625,#10626,#10627,#10628,#10629,#10630,
#10631,#10632,#10633,#10634,#10635,#10636,#10637,#10638));
#10966=CLOSED_SHELL('',(#10639,#10640,#10641,#10642,#10643,#10644,#10645,
#10646,#10647,#10648));
#10967=CLOSED_SHELL('',(#10649,#10650,#10651,#10652,#10653,#10654,#10655,
#10656,#10657,#10658,#10659,#10660,#10661,#10662));
#10968=CLOSED_SHELL('',(#10663,#10664,#10665,#10666,#10667,#10668,#10669,
#10670,#10671,#10672,#10673,#10674,#10675,#10676,#10677,#10678,#10679,#10680,
#10681,#10682,#10683,#10684,#10685,#10686,#10687,#10688,#10689,#10690,#10691,
#10692,#10693,#10694,#10695,#10696,#10697,#10698,#10699,#10700,#10701,#10702,
#10703,#10704,#10705,#10706,#10707,#10708,#10709,#10710,#10711,#10712,#10713,
#10714,#10715,#10716,#10717,#10718,#10719,#10720,#10721,#10722,#10723,#10724,
#10725,#10726,#10727,#10728,#10729,#10730,#10731,#10732,#10733,#10734,#10735,
#10736,#10737,#10738,#10739,#10740,#10741,#10742,#10743,#10744,#10745,#10746,
#10747,#10748,#10749,#10750,#10751,#10752,#10753,#10754,#10755,#10756,#10757,
#10758,#10759,#10760,#10761,#10762,#10763,#10764,#10765,#10766,#10767,#10768,
#10769,#10770,#10771,#10772,#10773,#10774,#10775,#10776,#10777,#10778,#10779,
#10780,#10781,#10782,#10783,#10784,#10785,#10786,#10787,#10788,#10789,#10790,
#10791,#10792,#10793,#10794,#10795,#10796,#10797,#10798,#10799,#10800,#10801,
#10802,#10803,#10804,#10805,#10806,#10807,#10808,#10809,#10810,#10811,#10812,
#10813,#10814,#10815,#10816,#10817,#10818,#10819,#10820,#10821,#10822,#10823,
#10824,#10825,#10826,#10827,#10828));
#10969=CLOSED_SHELL('',(#10829,#10830,#10831,#10832,#10833,#10834,#10835,
#10836,#10837,#10838,#10839,#10840,#10841,#10842,#10843,#10844,#10845,#10846,
#10847,#10848,#10849,#10850,#10851,#10852,#10853,#10854,#10855,#10856,#10857,
#10858,#10859,#10860,#10861,#10862,#10863,#10864));
#10970=CLOSED_SHELL('',(#10865,#10866,#10867,#10868,#10869,#10870,#10871,
#10872,#10873,#10874,#10875,#10876,#10877,#10878,#10879,#10880,#10881,#10882,
#10883));
#10971=CLOSED_SHELL('',(#10884,#10885,#10886,#10887,#10888,#10889,#10890,
#10891,#10892,#10893,#10894,#10895,#10896,#10897));
#10972=CLOSED_SHELL('',(#10898,#10899,#10900,#10901,#10902,#10903,#10904,
#10905,#10906,#10907,#10908,#10909,#10910));
#10973=CLOSED_SHELL('',(#10911));
#10974=CLOSED_SHELL('',(#10912));
#10975=CLOSED_SHELL('',(#10913));
#10976=CLOSED_SHELL('',(#10914));
#10977=CLOSED_SHELL('',(#10915));
#10978=CLOSED_SHELL('',(#10916));
#10979=CLOSED_SHELL('',(#10917));
#10980=CLOSED_SHELL('',(#10918,#10919,#10920,#10921,#10922,#10923,#10924,
#10925,#10926,#10927,#10928,#10929,#10930,#10931));
#10981=CLOSED_SHELL('',(#10932,#10933,#10934,#10935,#10936,#10937,#10938,
#10939,#10940,#10941,#10942,#10943,#10944,#10945,#10946,#10947,#10948,#10949,
#10950,#10951,#10952,#10953,#10954,#10955,#10956,#10957));
#10982=DERIVED_UNIT_ELEMENT(#11014,1.);
#10983=DERIVED_UNIT_ELEMENT(#18869,-3.);
#10984=DERIVED_UNIT_ELEMENT(#11014,1.);
#10985=DERIVED_UNIT_ELEMENT(#18869,-3.);
#10986=DERIVED_UNIT_ELEMENT(#11014,1.);
#10987=DERIVED_UNIT_ELEMENT(#18869,-3.);
#10988=DERIVED_UNIT_ELEMENT(#11014,1.);
#10989=DERIVED_UNIT_ELEMENT(#18869,-3.);
#10990=DERIVED_UNIT_ELEMENT(#11014,1.);
#10991=DERIVED_UNIT_ELEMENT(#18869,-3.);
#10992=DERIVED_UNIT_ELEMENT(#11014,1.);
#10993=DERIVED_UNIT_ELEMENT(#18869,-3.);
#10994=DERIVED_UNIT_ELEMENT(#11014,1.);
#10995=DERIVED_UNIT_ELEMENT(#18869,-3.);
#10996=DERIVED_UNIT_ELEMENT(#11014,1.);
#10997=DERIVED_UNIT_ELEMENT(#18869,-3.);
#10998=DERIVED_UNIT_ELEMENT(#11014,1.);
#10999=DERIVED_UNIT_ELEMENT(#18869,-3.);
#11000=DERIVED_UNIT_ELEMENT(#11014,1.);
#11001=DERIVED_UNIT_ELEMENT(#18869,-3.);
#11002=DERIVED_UNIT_ELEMENT(#11014,1.);
#11003=DERIVED_UNIT_ELEMENT(#18869,-3.);
#11004=DERIVED_UNIT_ELEMENT(#11014,1.);
#11005=DERIVED_UNIT_ELEMENT(#18869,-3.);
#11006=DERIVED_UNIT_ELEMENT(#11014,1.);
#11007=DERIVED_UNIT_ELEMENT(#18869,-3.);
#11008=DERIVED_UNIT_ELEMENT(#11014,1.);
#11009=DERIVED_UNIT_ELEMENT(#18869,-3.);
#11010=DERIVED_UNIT_ELEMENT(#11014,1.);
#11011=DERIVED_UNIT_ELEMENT(#18869,-3.);
#11012=DERIVED_UNIT_ELEMENT(#11014,1.);
#11013=DERIVED_UNIT_ELEMENT(#18869,-3.);
#11014=(
MASS_UNIT()
NAMED_UNIT(*)
SI_UNIT(.KILO.,.GRAM.)
);
#11015=DERIVED_UNIT((#10982,#10983));
#11016=DERIVED_UNIT((#10984,#10985));
#11017=DERIVED_UNIT((#10986,#10987));
#11018=DERIVED_UNIT((#10988,#10989));
#11019=DERIVED_UNIT((#10990,#10991));
#11020=DERIVED_UNIT((#10992,#10993));
#11021=DERIVED_UNIT((#10994,#10995));
#11022=DERIVED_UNIT((#10996,#10997));
#11023=DERIVED_UNIT((#10998,#10999));
#11024=DERIVED_UNIT((#11000,#11001));
#11025=DERIVED_UNIT((#11002,#11003));
#11026=DERIVED_UNIT((#11004,#11005));
#11027=DERIVED_UNIT((#11006,#11007));
#11028=DERIVED_UNIT((#11008,#11009));
#11029=DERIVED_UNIT((#11010,#11011));
#11030=DERIVED_UNIT((#11012,#11013));
#11031=MEASURE_REPRESENTATION_ITEM('density measure',
POSITIVE_RATIO_MEASURE(7850.),#11015);
#11032=MEASURE_REPRESENTATION_ITEM('density measure',
POSITIVE_RATIO_MEASURE(7850.),#11016);
#11033=MEASURE_REPRESENTATION_ITEM('density measure',
POSITIVE_RATIO_MEASURE(7850.),#11017);
#11034=MEASURE_REPRESENTATION_ITEM('density measure',
POSITIVE_RATIO_MEASURE(7850.),#11018);
#11035=MEASURE_REPRESENTATION_ITEM('density measure',
POSITIVE_RATIO_MEASURE(7850.),#11019);
#11036=MEASURE_REPRESENTATION_ITEM('density measure',
POSITIVE_RATIO_MEASURE(7850.),#11020);
#11037=MEASURE_REPRESENTATION_ITEM('density measure',
POSITIVE_RATIO_MEASURE(7850.),#11021);
#11038=MEASURE_REPRESENTATION_ITEM('density measure',
POSITIVE_RATIO_MEASURE(7850.),#11022);
#11039=MEASURE_REPRESENTATION_ITEM('density measure',
POSITIVE_RATIO_MEASURE(7850.),#11023);
#11040=MEASURE_REPRESENTATION_ITEM('density measure',
POSITIVE_RATIO_MEASURE(7850.),#11024);
#11041=MEASURE_REPRESENTATION_ITEM('density measure',
POSITIVE_RATIO_MEASURE(7850.),#11025);
#11042=MEASURE_REPRESENTATION_ITEM('density measure',
POSITIVE_RATIO_MEASURE(7850.),#11026);
#11043=MEASURE_REPRESENTATION_ITEM('density measure',
POSITIVE_RATIO_MEASURE(7850.),#11027);
#11044=MEASURE_REPRESENTATION_ITEM('density measure',
POSITIVE_RATIO_MEASURE(7850.),#11028);
#11045=MEASURE_REPRESENTATION_ITEM('density measure',
POSITIVE_RATIO_MEASURE(7850.),#11029);
#11046=MEASURE_REPRESENTATION_ITEM('density measure',
POSITIVE_RATIO_MEASURE(7850.),#11030);
#11047=PROPERTY_DEFINITION_REPRESENTATION(#11127,#11079);
#11048=PROPERTY_DEFINITION_REPRESENTATION(#11128,#11080);
#11049=PROPERTY_DEFINITION_REPRESENTATION(#11129,#11081);
#11050=PROPERTY_DEFINITION_REPRESENTATION(#11130,#11082);
#11051=PROPERTY_DEFINITION_REPRESENTATION(#11131,#11083);
#11052=PROPERTY_DEFINITION_REPRESENTATION(#11132,#11084);
#11053=PROPERTY_DEFINITION_REPRESENTATION(#11133,#11085);
#11054=PROPERTY_DEFINITION_REPRESENTATION(#11134,#11086);
#11055=PROPERTY_DEFINITION_REPRESENTATION(#11135,#11087);
#11056=PROPERTY_DEFINITION_REPRESENTATION(#11136,#11088);
#11057=PROPERTY_DEFINITION_REPRESENTATION(#11137,#11089);
#11058=PROPERTY_DEFINITION_REPRESENTATION(#11138,#11090);
#11059=PROPERTY_DEFINITION_REPRESENTATION(#11139,#11091);
#11060=PROPERTY_DEFINITION_REPRESENTATION(#11140,#11092);
#11061=PROPERTY_DEFINITION_REPRESENTATION(#11141,#11093);
#11062=PROPERTY_DEFINITION_REPRESENTATION(#11142,#11094);
#11063=PROPERTY_DEFINITION_REPRESENTATION(#11143,#11095);
#11064=PROPERTY_DEFINITION_REPRESENTATION(#11144,#11096);
#11065=PROPERTY_DEFINITION_REPRESENTATION(#11145,#11097);
#11066=PROPERTY_DEFINITION_REPRESENTATION(#11146,#11098);
#11067=PROPERTY_DEFINITION_REPRESENTATION(#11147,#11099);
#11068=PROPERTY_DEFINITION_REPRESENTATION(#11148,#11100);
#11069=PROPERTY_DEFINITION_REPRESENTATION(#11149,#11101);
#11070=PROPERTY_DEFINITION_REPRESENTATION(#11150,#11102);
#11071=PROPERTY_DEFINITION_REPRESENTATION(#11151,#11103);
#11072=PROPERTY_DEFINITION_REPRESENTATION(#11152,#11104);
#11073=PROPERTY_DEFINITION_REPRESENTATION(#11153,#11105);
#11074=PROPERTY_DEFINITION_REPRESENTATION(#11154,#11106);
#11075=PROPERTY_DEFINITION_REPRESENTATION(#11155,#11107);
#11076=PROPERTY_DEFINITION_REPRESENTATION(#11156,#11108);
#11077=PROPERTY_DEFINITION_REPRESENTATION(#11157,#11109);
#11078=PROPERTY_DEFINITION_REPRESENTATION(#11158,#11110);
#11079=REPRESENTATION('material name',(#11111),#18851);
#11080=REPRESENTATION('density',(#11031),#18851);
#11081=REPRESENTATION('material name',(#11112),#18852);
#11082=REPRESENTATION('density',(#11032),#18852);
#11083=REPRESENTATION('material name',(#11113),#18853);
#11084=REPRESENTATION('density',(#11033),#18853);
#11085=REPRESENTATION('material name',(#11114),#18854);
#11086=REPRESENTATION('density',(#11034),#18854);
#11087=REPRESENTATION('material name',(#11115),#18855);
#11088=REPRESENTATION('density',(#11035),#18855);
#11089=REPRESENTATION('material name',(#11116),#18856);
#11090=REPRESENTATION('density',(#11036),#18856);
#11091=REPRESENTATION('material name',(#11117),#18857);
#11092=REPRESENTATION('density',(#11037),#18857);
#11093=REPRESENTATION('material name',(#11118),#18858);
#11094=REPRESENTATION('density',(#11038),#18858);
#11095=REPRESENTATION('material name',(#11119),#18859);
#11096=REPRESENTATION('density',(#11039),#18859);
#11097=REPRESENTATION('material name',(#11120),#18860);
#11098=REPRESENTATION('density',(#11040),#18860);
#11099=REPRESENTATION('material name',(#11121),#18861);
#11100=REPRESENTATION('density',(#11041),#18861);
#11101=REPRESENTATION('material name',(#11122),#18862);
#11102=REPRESENTATION('density',(#11042),#18862);
#11103=REPRESENTATION('material name',(#11123),#18863);
#11104=REPRESENTATION('density',(#11043),#18863);
#11105=REPRESENTATION('material name',(#11124),#18864);
#11106=REPRESENTATION('density',(#11044),#18864);
#11107=REPRESENTATION('material name',(#11125),#18865);
#11108=REPRESENTATION('density',(#11045),#18865);
#11109=REPRESENTATION('material name',(#11126),#18866);
#11110=REPRESENTATION('density',(#11046),#18866);
#11111=DESCRIPTIVE_REPRESENTATION_ITEM('Steel','Steel');
#11112=DESCRIPTIVE_REPRESENTATION_ITEM('Steel','Steel');
#11113=DESCRIPTIVE_REPRESENTATION_ITEM('Steel','Steel');
#11114=DESCRIPTIVE_REPRESENTATION_ITEM('Steel','Steel');
#11115=DESCRIPTIVE_REPRESENTATION_ITEM('Steel','Steel');
#11116=DESCRIPTIVE_REPRESENTATION_ITEM('Steel','Steel');
#11117=DESCRIPTIVE_REPRESENTATION_ITEM('Steel','Steel');
#11118=DESCRIPTIVE_REPRESENTATION_ITEM('Steel','Steel');
#11119=DESCRIPTIVE_REPRESENTATION_ITEM('Steel','Steel');
#11120=DESCRIPTIVE_REPRESENTATION_ITEM('Steel','Steel');
#11121=DESCRIPTIVE_REPRESENTATION_ITEM('Steel','Steel');
#11122=DESCRIPTIVE_REPRESENTATION_ITEM('Steel','Steel');
#11123=DESCRIPTIVE_REPRESENTATION_ITEM('Steel','Steel');
#11124=DESCRIPTIVE_REPRESENTATION_ITEM('Steel','Steel');
#11125=DESCRIPTIVE_REPRESENTATION_ITEM('Steel','Steel');
#11126=DESCRIPTIVE_REPRESENTATION_ITEM('Steel','Steel');
#11127=PROPERTY_DEFINITION('material property','material name',#18953);
#11128=PROPERTY_DEFINITION('material property','density of part',#18953);
#11129=PROPERTY_DEFINITION('material property','material name',#18954);
#11130=PROPERTY_DEFINITION('material property','density of part',#18954);
#11131=PROPERTY_DEFINITION('material property','material name',#18955);
#11132=PROPERTY_DEFINITION('material property','density of part',#18955);
#11133=PROPERTY_DEFINITION('material property','material name',#18956);
#11134=PROPERTY_DEFINITION('material property','density of part',#18956);
#11135=PROPERTY_DEFINITION('material property','material name',#18957);
#11136=PROPERTY_DEFINITION('material property','density of part',#18957);
#11137=PROPERTY_DEFINITION('material property','material name',#18958);
#11138=PROPERTY_DEFINITION('material property','density of part',#18958);
#11139=PROPERTY_DEFINITION('material property','material name',#18959);
#11140=PROPERTY_DEFINITION('material property','density of part',#18959);
#11141=PROPERTY_DEFINITION('material property','material name',#18960);
#11142=PROPERTY_DEFINITION('material property','density of part',#18960);
#11143=PROPERTY_DEFINITION('material property','material name',#18961);
#11144=PROPERTY_DEFINITION('material property','density of part',#18961);
#11145=PROPERTY_DEFINITION('material property','material name',#18962);
#11146=PROPERTY_DEFINITION('material property','density of part',#18962);
#11147=PROPERTY_DEFINITION('material property','material name',#18963);
#11148=PROPERTY_DEFINITION('material property','density of part',#18963);
#11149=PROPERTY_DEFINITION('material property','material name',#18964);
#11150=PROPERTY_DEFINITION('material property','density of part',#18964);
#11151=PROPERTY_DEFINITION('material property','material name',#18965);
#11152=PROPERTY_DEFINITION('material property','density of part',#18965);
#11153=PROPERTY_DEFINITION('material property','material name',#18966);
#11154=PROPERTY_DEFINITION('material property','density of part',#18966);
#11155=PROPERTY_DEFINITION('material property','material name',#18967);
#11156=PROPERTY_DEFINITION('material property','density of part',#18967);
#11157=PROPERTY_DEFINITION('material property','material name',#18968);
#11158=PROPERTY_DEFINITION('material property','density of part',#18968);
#11159=AXIS2_PLACEMENT_3D('',#15605,#12303,#12304);
#11160=AXIS2_PLACEMENT_3D('',#15606,#12305,#12306);
#11161=AXIS2_PLACEMENT_3D('',#15607,#12307,#12308);
#11162=AXIS2_PLACEMENT_3D('',#15609,#12309,#12310);
#11163=AXIS2_PLACEMENT_3D('',#15612,#12312,#12313);
#11164=AXIS2_PLACEMENT_3D('',#15613,#12314,#12315);
#11165=AXIS2_PLACEMENT_3D('',#15615,#12316,#12317);
#11166=AXIS2_PLACEMENT_3D('',#15618,#12319,#12320);
#11167=AXIS2_PLACEMENT_3D('',#15619,#12321,#12322);
#11168=AXIS2_PLACEMENT_3D('',#15621,#12323,#12324);
#11169=AXIS2_PLACEMENT_3D('',#15624,#12326,#12327);
#11170=AXIS2_PLACEMENT_3D('',#15625,#12328,#12329);
#11171=AXIS2_PLACEMENT_3D('',#15627,#12330,#12331);
#11172=AXIS2_PLACEMENT_3D('',#15630,#12333,#12334);
#11173=AXIS2_PLACEMENT_3D('',#15631,#12335,#12336);
#11174=AXIS2_PLACEMENT_3D('',#15633,#12337,#12338);
#11175=AXIS2_PLACEMENT_3D('',#15636,#12340,#12341);
#11176=AXIS2_PLACEMENT_3D('',#15637,#12342,#12343);
#11177=AXIS2_PLACEMENT_3D('',#15639,#12344,#12345);
#11178=AXIS2_PLACEMENT_3D('',#15642,#12347,#12348);
#11179=AXIS2_PLACEMENT_3D('',#15643,#12349,#12350);
#11180=AXIS2_PLACEMENT_3D('',#15645,#12351,#12352);
#11181=AXIS2_PLACEMENT_3D('',#15648,#12354,#12355);
#11182=AXIS2_PLACEMENT_3D('',#15649,#12356,#12357);
#11183=AXIS2_PLACEMENT_3D('',#15651,#12358,#12359);
#11184=AXIS2_PLACEMENT_3D('',#15654,#12361,#12362);
#11185=AXIS2_PLACEMENT_3D('',#15655,#12363,#12364);
#11186=AXIS2_PLACEMENT_3D('',#15657,#12365,#12366);
#11187=AXIS2_PLACEMENT_3D('',#15660,#12368,#12369);
#11188=AXIS2_PLACEMENT_3D('',#15661,#12370,#12371);
#11189=AXIS2_PLACEMENT_3D('',#15682,#12382,#12383);
#11190=AXIS2_PLACEMENT_3D('',#15688,#12386,#12387);
#11191=AXIS2_PLACEMENT_3D('',#15690,#12389,#12390);
#11192=AXIS2_PLACEMENT_3D('',#15696,#12393,#12394);
#11193=AXIS2_PLACEMENT_3D('',#15698,#12396,#12397);
#11194=AXIS2_PLACEMENT_3D('',#15709,#12402,#12403);
#11195=AXIS2_PLACEMENT_3D('',#15738,#12419,#12420);
#11196=AXIS2_PLACEMENT_3D('',#15744,#12424,#12425);
#11197=AXIS2_PLACEMENT_3D('',#15747,#12427,#12428);
#11198=AXIS2_PLACEMENT_3D('',#15748,#12429,#12430);
#11199=AXIS2_PLACEMENT_3D('',#15755,#12435,#12436);
#11200=AXIS2_PLACEMENT_3D('',#15766,#12443,#12444);
#11201=AXIS2_PLACEMENT_3D('',#15770,#12447,#12448);
#11202=AXIS2_PLACEMENT_3D('',#15771,#12449,#12450);
#11203=AXIS2_PLACEMENT_3D('',#15772,#12451,#12452);
#11204=AXIS2_PLACEMENT_3D('',#15773,#12453,#12454);
#11205=AXIS2_PLACEMENT_3D('',#15774,#12455,#12456);
#11206=AXIS2_PLACEMENT_3D('',#15775,#12457,#12458);
#11207=AXIS2_PLACEMENT_3D('',#15779,#12461,#12462);
#11208=AXIS2_PLACEMENT_3D('',#15783,#12465,#12466);
#11209=AXIS2_PLACEMENT_3D('',#15789,#12470,#12471);
#11210=AXIS2_PLACEMENT_3D('',#15790,#12472,#12473);
#11211=AXIS2_PLACEMENT_3D('',#15791,#12474,#12475);
#11212=AXIS2_PLACEMENT_3D('',#15792,#12476,#12477);
#11213=AXIS2_PLACEMENT_3D('',#15793,#12478,#12479);
#11214=AXIS2_PLACEMENT_3D('',#15799,#12483,#12484);
#11215=AXIS2_PLACEMENT_3D('',#15803,#12487,#12488);
#11216=AXIS2_PLACEMENT_3D('',#15807,#12491,#12492);
#11217=AXIS2_PLACEMENT_3D('',#15811,#12495,#12496);
#11218=AXIS2_PLACEMENT_3D('',#15815,#12499,#12500);
#11219=AXIS2_PLACEMENT_3D('',#15817,#12502,#12503);
#11220=AXIS2_PLACEMENT_3D('',#15818,#12504,#12505);
#11221=AXIS2_PLACEMENT_3D('',#15824,#12509,#12510);
#11222=AXIS2_PLACEMENT_3D('',#15828,#12513,#12514);
#11223=AXIS2_PLACEMENT_3D('',#15832,#12517,#12518);
#11224=AXIS2_PLACEMENT_3D('',#15836,#12521,#12522);
#11225=AXIS2_PLACEMENT_3D('',#15840,#12525,#12526);
#11226=AXIS2_PLACEMENT_3D('',#15842,#12528,#12529);
#11227=AXIS2_PLACEMENT_3D('',#15843,#12530,#12531);
#11228=AXIS2_PLACEMENT_3D('',#15845,#12533,#12534);
#11229=AXIS2_PLACEMENT_3D('',#15847,#12536,#12537);
#11230=AXIS2_PLACEMENT_3D('',#15848,#12538,#12539);
#11231=AXIS2_PLACEMENT_3D('',#15851,#12542,#12543);
#11232=AXIS2_PLACEMENT_3D('',#15852,#12544,#12545);
#11233=AXIS2_PLACEMENT_3D('',#15853,#12546,#12547);
#11234=AXIS2_PLACEMENT_3D('',#15854,#12548,#12549);
#11235=AXIS2_PLACEMENT_3D('',#15856,#12550,#12551);
#11236=AXIS2_PLACEMENT_3D('',#15859,#12553,#12554);
#11237=AXIS2_PLACEMENT_3D('',#15860,#12555,#12556);
#11238=AXIS2_PLACEMENT_3D('',#15862,#12557,#12558);
#11239=AXIS2_PLACEMENT_3D('',#15865,#12560,#12561);
#11240=AXIS2_PLACEMENT_3D('',#15866,#12562,#12563);
#11241=AXIS2_PLACEMENT_3D('',#15868,#12564,#12565);
#11242=AXIS2_PLACEMENT_3D('',#15871,#12567,#12568);
#11243=AXIS2_PLACEMENT_3D('',#15872,#12569,#12570);
#11244=AXIS2_PLACEMENT_3D('',#15874,#12571,#12572);
#11245=AXIS2_PLACEMENT_3D('',#15877,#12574,#12575);
#11246=AXIS2_PLACEMENT_3D('',#15878,#12576,#12577);
#11247=AXIS2_PLACEMENT_3D('',#15880,#12578,#12579);
#11248=AXIS2_PLACEMENT_3D('',#15883,#12581,#12582);
#11249=AXIS2_PLACEMENT_3D('',#15884,#12583,#12584);
#11250=AXIS2_PLACEMENT_3D('',#15886,#12585,#12586);
#11251=AXIS2_PLACEMENT_3D('',#15889,#12588,#12589);
#11252=AXIS2_PLACEMENT_3D('',#15890,#12590,#12591);
#11253=AXIS2_PLACEMENT_3D('',#15892,#12592,#12593);
#11254=AXIS2_PLACEMENT_3D('',#15895,#12595,#12596);
#11255=AXIS2_PLACEMENT_3D('',#15896,#12597,#12598);
#11256=AXIS2_PLACEMENT_3D('',#15898,#12599,#12600);
#11257=AXIS2_PLACEMENT_3D('',#15901,#12602,#12603);
#11258=AXIS2_PLACEMENT_3D('',#15902,#12604,#12605);
#11259=AXIS2_PLACEMENT_3D('',#15904,#12606,#12607);
#11260=AXIS2_PLACEMENT_3D('',#15907,#12609,#12610);
#11261=AXIS2_PLACEMENT_3D('',#15908,#12611,#12612);
#11262=AXIS2_PLACEMENT_3D('',#15929,#12623,#12624);
#11263=AXIS2_PLACEMENT_3D('',#15935,#12627,#12628);
#11264=AXIS2_PLACEMENT_3D('',#15937,#12630,#12631);
#11265=AXIS2_PLACEMENT_3D('',#15943,#12634,#12635);
#11266=AXIS2_PLACEMENT_3D('',#15945,#12637,#12638);
#11267=AXIS2_PLACEMENT_3D('',#15955,#12643,#12644);
#11268=AXIS2_PLACEMENT_3D('',#15985,#12660,#12661);
#11269=AXIS2_PLACEMENT_3D('',#15991,#12665,#12666);
#11270=AXIS2_PLACEMENT_3D('',#15993,#12667,#12668);
#11271=AXIS2_PLACEMENT_3D('',#15995,#12670,#12671);
#11272=AXIS2_PLACEMENT_3D('',#16002,#12676,#12677);
#11273=AXIS2_PLACEMENT_3D('',#16013,#12684,#12685);
#11274=AXIS2_PLACEMENT_3D('',#16017,#12688,#12689);
#11275=AXIS2_PLACEMENT_3D('',#16018,#12690,#12691);
#11276=AXIS2_PLACEMENT_3D('',#16019,#12692,#12693);
#11277=AXIS2_PLACEMENT_3D('',#16020,#12694,#12695);
#11278=AXIS2_PLACEMENT_3D('',#16021,#12696,#12697);
#11279=AXIS2_PLACEMENT_3D('',#16022,#12698,#12699);
#11280=AXIS2_PLACEMENT_3D('',#16026,#12702,#12703);
#11281=AXIS2_PLACEMENT_3D('',#16030,#12706,#12707);
#11282=AXIS2_PLACEMENT_3D('',#16036,#12711,#12712);
#11283=AXIS2_PLACEMENT_3D('',#16037,#12713,#12714);
#11284=AXIS2_PLACEMENT_3D('',#16038,#12715,#12716);
#11285=AXIS2_PLACEMENT_3D('',#16039,#12717,#12718);
#11286=AXIS2_PLACEMENT_3D('',#16040,#12719,#12720);
#11287=AXIS2_PLACEMENT_3D('',#16046,#12724,#12725);
#11288=AXIS2_PLACEMENT_3D('',#16050,#12728,#12729);
#11289=AXIS2_PLACEMENT_3D('',#16054,#12732,#12733);
#11290=AXIS2_PLACEMENT_3D('',#16058,#12736,#12737);
#11291=AXIS2_PLACEMENT_3D('',#16062,#12740,#12741);
#11292=AXIS2_PLACEMENT_3D('',#16064,#12743,#12744);
#11293=AXIS2_PLACEMENT_3D('',#16065,#12745,#12746);
#11294=AXIS2_PLACEMENT_3D('',#16071,#12750,#12751);
#11295=AXIS2_PLACEMENT_3D('',#16075,#12754,#12755);
#11296=AXIS2_PLACEMENT_3D('',#16079,#12758,#12759);
#11297=AXIS2_PLACEMENT_3D('',#16083,#12762,#12763);
#11298=AXIS2_PLACEMENT_3D('',#16087,#12766,#12767);
#11299=AXIS2_PLACEMENT_3D('',#16089,#12769,#12770);
#11300=AXIS2_PLACEMENT_3D('',#16090,#12771,#12772);
#11301=AXIS2_PLACEMENT_3D('',#16092,#12774,#12775);
#11302=AXIS2_PLACEMENT_3D('',#16094,#12777,#12778);
#11303=AXIS2_PLACEMENT_3D('',#16095,#12779,#12780);
#11304=AXIS2_PLACEMENT_3D('',#16098,#12783,#12784);
#11305=AXIS2_PLACEMENT_3D('',#16099,#12785,#12786);
#11306=AXIS2_PLACEMENT_3D('',#16100,#12787,#12788);
#11307=AXIS2_PLACEMENT_3D('',#16101,#12789,#12790);
#11308=AXIS2_PLACEMENT_3D('',#16103,#12791,#12792);
#11309=AXIS2_PLACEMENT_3D('',#16107,#12794,#12795);
#11310=AXIS2_PLACEMENT_3D('',#16109,#12796,#12797);
#11311=AXIS2_PLACEMENT_3D('',#16110,#12798,#12799);
#11312=AXIS2_PLACEMENT_3D('',#16111,#12800,#12801);
#11313=AXIS2_PLACEMENT_3D('',#16113,#12802,#12803);
#11314=AXIS2_PLACEMENT_3D('',#16116,#12805,#12806);
#11315=AXIS2_PLACEMENT_3D('',#16117,#12807,#12808);
#11316=AXIS2_PLACEMENT_3D('',#16119,#12809,#12810);
#11317=AXIS2_PLACEMENT_3D('',#16122,#12812,#12813);
#11318=AXIS2_PLACEMENT_3D('',#16123,#12814,#12815);
#11319=AXIS2_PLACEMENT_3D('',#16125,#12816,#12817);
#11320=AXIS2_PLACEMENT_3D('',#16128,#12819,#12820);
#11321=AXIS2_PLACEMENT_3D('',#16129,#12821,#12822);
#11322=AXIS2_PLACEMENT_3D('',#16131,#12823,#12824);
#11323=AXIS2_PLACEMENT_3D('',#16134,#12826,#12827);
#11324=AXIS2_PLACEMENT_3D('',#16135,#12828,#12829);
#11325=AXIS2_PLACEMENT_3D('',#16137,#12830,#12831);
#11326=AXIS2_PLACEMENT_3D('',#16140,#12833,#12834);
#11327=AXIS2_PLACEMENT_3D('',#16141,#12835,#12836);
#11328=AXIS2_PLACEMENT_3D('',#16143,#12837,#12838);
#11329=AXIS2_PLACEMENT_3D('',#16146,#12840,#12841);
#11330=AXIS2_PLACEMENT_3D('',#16147,#12842,#12843);
#11331=AXIS2_PLACEMENT_3D('',#16156,#12847,#12848);
#11332=AXIS2_PLACEMENT_3D('',#16158,#12850,#12851);
#11333=AXIS2_PLACEMENT_3D('',#16165,#12854,#12855);
#11334=AXIS2_PLACEMENT_3D('',#16169,#12858,#12859);
#11335=AXIS2_PLACEMENT_3D('',#16180,#12866,#12867);
#11336=AXIS2_PLACEMENT_3D('',#16188,#12872,#12873);
#11337=AXIS2_PLACEMENT_3D('',#16190,#12874,#12875);
#11338=AXIS2_PLACEMENT_3D('',#16192,#12876,#12877);
#11339=AXIS2_PLACEMENT_3D('',#16194,#12879,#12880);
#11340=AXIS2_PLACEMENT_3D('',#16199,#12884,#12885);
#11341=AXIS2_PLACEMENT_3D('',#16207,#12889,#12890);
#11342=AXIS2_PLACEMENT_3D('',#16211,#12892,#12893);
#11343=AXIS2_PLACEMENT_3D('',#16222,#12900,#12901);
#11344=AXIS2_PLACEMENT_3D('',#16226,#12904,#12905);
#11345=AXIS2_PLACEMENT_3D('',#16229,#12907,#12908);
#11346=AXIS2_PLACEMENT_3D('',#16230,#12909,#12910);
#11347=AXIS2_PLACEMENT_3D('',#16235,#12914,#12915);
#11348=AXIS2_PLACEMENT_3D('',#16236,#12916,#12917);
#11349=AXIS2_PLACEMENT_3D('',#16237,#12918,#12919);
#11350=AXIS2_PLACEMENT_3D('',#16238,#12920,#12921);
#11351=AXIS2_PLACEMENT_3D('',#16239,#12922,#12923);
#11352=AXIS2_PLACEMENT_3D('',#16240,#12924,#12925);
#11353=AXIS2_PLACEMENT_3D('',#16241,#12926,#12927);
#11354=AXIS2_PLACEMENT_3D('',#16242,#12928,#12929);
#11355=AXIS2_PLACEMENT_3D('',#16248,#12933,#12934);
#11356=AXIS2_PLACEMENT_3D('',#16250,#12935,#12936);
#11357=AXIS2_PLACEMENT_3D('',#16254,#12938,#12939);
#11358=AXIS2_PLACEMENT_3D('',#16258,#12942,#12943);
#11359=AXIS2_PLACEMENT_3D('',#16261,#12946,#12947);
#11360=AXIS2_PLACEMENT_3D('',#16264,#12950,#12951);
#11361=AXIS2_PLACEMENT_3D('',#16265,#12952,#12953);
#11362=AXIS2_PLACEMENT_3D('',#16266,#12954,#12955);
#11363=AXIS2_PLACEMENT_3D('',#16267,#12956,#12957);
#11364=AXIS2_PLACEMENT_3D('',#16270,#12960,#12961);
#11365=AXIS2_PLACEMENT_3D('',#16271,#12962,#12963);
#11366=AXIS2_PLACEMENT_3D('',#16272,#12964,#12965);
#11367=AXIS2_PLACEMENT_3D('',#16273,#12966,#12967);
#11368=AXIS2_PLACEMENT_3D('',#16275,#12968,#12969);
#11369=AXIS2_PLACEMENT_3D('',#16279,#12971,#12972);
#11370=AXIS2_PLACEMENT_3D('',#16281,#12973,#12974);
#11371=AXIS2_PLACEMENT_3D('',#16282,#12975,#12976);
#11372=AXIS2_PLACEMENT_3D('',#16283,#12977,#12978);
#11373=AXIS2_PLACEMENT_3D('',#16285,#12979,#12980);
#11374=AXIS2_PLACEMENT_3D('',#16288,#12982,#12983);
#11375=AXIS2_PLACEMENT_3D('',#16289,#12984,#12985);
#11376=AXIS2_PLACEMENT_3D('',#16291,#12986,#12987);
#11377=AXIS2_PLACEMENT_3D('',#16294,#12989,#12990);
#11378=AXIS2_PLACEMENT_3D('',#16295,#12991,#12992);
#11379=AXIS2_PLACEMENT_3D('',#16297,#12993,#12994);
#11380=AXIS2_PLACEMENT_3D('',#16300,#12996,#12997);
#11381=AXIS2_PLACEMENT_3D('',#16301,#12998,#12999);
#11382=AXIS2_PLACEMENT_3D('',#16303,#13000,#13001);
#11383=AXIS2_PLACEMENT_3D('',#16306,#13003,#13004);
#11384=AXIS2_PLACEMENT_3D('',#16307,#13005,#13006);
#11385=AXIS2_PLACEMENT_3D('',#16309,#13007,#13008);
#11386=AXIS2_PLACEMENT_3D('',#16312,#13010,#13011);
#11387=AXIS2_PLACEMENT_3D('',#16313,#13012,#13013);
#11388=AXIS2_PLACEMENT_3D('',#16315,#13014,#13015);
#11389=AXIS2_PLACEMENT_3D('',#16318,#13017,#13018);
#11390=AXIS2_PLACEMENT_3D('',#16319,#13019,#13020);
#11391=AXIS2_PLACEMENT_3D('',#16326,#13023,#13024);
#11392=AXIS2_PLACEMENT_3D('',#16330,#13027,#13028);
#11393=AXIS2_PLACEMENT_3D('',#16339,#13032,#13033);
#11394=AXIS2_PLACEMENT_3D('',#16341,#13035,#13036);
#11395=AXIS2_PLACEMENT_3D('',#16352,#13043,#13044);
#11396=AXIS2_PLACEMENT_3D('',#16360,#13049,#13050);
#11397=AXIS2_PLACEMENT_3D('',#16362,#13051,#13052);
#11398=AXIS2_PLACEMENT_3D('',#16365,#13054,#13055);
#11399=AXIS2_PLACEMENT_3D('',#16366,#13056,#13057);
#11400=AXIS2_PLACEMENT_3D('',#16371,#13061,#13062);
#11401=AXIS2_PLACEMENT_3D('',#16386,#13070,#13071);
#11402=AXIS2_PLACEMENT_3D('',#16390,#13073,#13074);
#11403=AXIS2_PLACEMENT_3D('',#16394,#13077,#13078);
#11404=AXIS2_PLACEMENT_3D('',#16398,#13081,#13082);
#11405=AXIS2_PLACEMENT_3D('',#16405,#13087,#13088);
#11406=AXIS2_PLACEMENT_3D('',#16406,#13089,#13090);
#11407=AXIS2_PLACEMENT_3D('',#16407,#13091,#13092);
#11408=AXIS2_PLACEMENT_3D('',#16408,#13093,#13094);
#11409=AXIS2_PLACEMENT_3D('',#16409,#13095,#13096);
#11410=AXIS2_PLACEMENT_3D('',#16410,#13097,#13098);
#11411=AXIS2_PLACEMENT_3D('',#16411,#13099,#13100);
#11412=AXIS2_PLACEMENT_3D('',#16412,#13101,#13102);
#11413=AXIS2_PLACEMENT_3D('',#16413,#13103,#13104);
#11414=AXIS2_PLACEMENT_3D('',#16414,#13105,#13106);
#11415=AXIS2_PLACEMENT_3D('',#16420,#13110,#13111);
#11416=AXIS2_PLACEMENT_3D('',#16426,#13114,#13115);
#11417=AXIS2_PLACEMENT_3D('',#16429,#13117,#13118);
#11418=AXIS2_PLACEMENT_3D('',#16430,#13119,#13120);
#11419=AXIS2_PLACEMENT_3D('',#16433,#13123,#13124);
#11420=AXIS2_PLACEMENT_3D('',#16436,#13127,#13128);
#11421=AXIS2_PLACEMENT_3D('',#16437,#13129,#13130);
#11422=AXIS2_PLACEMENT_3D('',#16438,#13131,#13132);
#11423=AXIS2_PLACEMENT_3D('',#16439,#13133,#13134);
#11424=AXIS2_PLACEMENT_3D('',#16442,#13137,#13138);
#11425=AXIS2_PLACEMENT_3D('',#16443,#13139,#13140);
#11426=AXIS2_PLACEMENT_3D('',#16444,#13141,#13142);
#11427=AXIS2_PLACEMENT_3D('',#16445,#13143,#13144);
#11428=AXIS2_PLACEMENT_3D('',#16447,#13145,#13146);
#11429=AXIS2_PLACEMENT_3D('',#16450,#13148,#13149);
#11430=AXIS2_PLACEMENT_3D('',#16451,#13150,#13151);
#11431=AXIS2_PLACEMENT_3D('',#16453,#13152,#13153);
#11432=AXIS2_PLACEMENT_3D('',#16456,#13155,#13156);
#11433=AXIS2_PLACEMENT_3D('',#16457,#13157,#13158);
#11434=AXIS2_PLACEMENT_3D('',#16459,#13159,#13160);
#11435=AXIS2_PLACEMENT_3D('',#16462,#13162,#13163);
#11436=AXIS2_PLACEMENT_3D('',#16463,#13164,#13165);
#11437=AXIS2_PLACEMENT_3D('',#16465,#13166,#13167);
#11438=AXIS2_PLACEMENT_3D('',#16468,#13169,#13170);
#11439=AXIS2_PLACEMENT_3D('',#16469,#13171,#13172);
#11440=AXIS2_PLACEMENT_3D('',#16471,#13173,#13174);
#11441=AXIS2_PLACEMENT_3D('',#16474,#13176,#13177);
#11442=AXIS2_PLACEMENT_3D('',#16475,#13178,#13179);
#11443=AXIS2_PLACEMENT_3D('',#16477,#13180,#13181);
#11444=AXIS2_PLACEMENT_3D('',#16480,#13183,#13184);
#11445=AXIS2_PLACEMENT_3D('',#16481,#13185,#13186);
#11446=AXIS2_PLACEMENT_3D('',#16483,#13187,#13188);
#11447=AXIS2_PLACEMENT_3D('',#16486,#13190,#13191);
#11448=AXIS2_PLACEMENT_3D('',#16487,#13192,#13193);
#11449=AXIS2_PLACEMENT_3D('',#16489,#13194,#13195);
#11450=AXIS2_PLACEMENT_3D('',#16492,#13197,#13198);
#11451=AXIS2_PLACEMENT_3D('',#16493,#13199,#13200);
#11452=AXIS2_PLACEMENT_3D('',#16495,#13201,#13202);
#11453=AXIS2_PLACEMENT_3D('',#16498,#13204,#13205);
#11454=AXIS2_PLACEMENT_3D('',#16499,#13206,#13207);
#11455=AXIS2_PLACEMENT_3D('',#16501,#13208,#13209);
#11456=AXIS2_PLACEMENT_3D('',#16504,#13211,#13212);
#11457=AXIS2_PLACEMENT_3D('',#16505,#13213,#13214);
#11458=AXIS2_PLACEMENT_3D('',#16514,#13219,#13220);
#11459=AXIS2_PLACEMENT_3D('',#16523,#13225,#13226);
#11460=AXIS2_PLACEMENT_3D('',#16532,#13231,#13232);
#11461=AXIS2_PLACEMENT_3D('',#16533,#13233,#13234);
#11462=AXIS2_PLACEMENT_3D('',#16534,#13235,#13236);
#11463=AXIS2_PLACEMENT_3D('',#16535,#13237,#13238);
#11464=AXIS2_PLACEMENT_3D('',#16536,#13239,#13240);
#11465=AXIS2_PLACEMENT_3D('',#16537,#13241,#13242);
#11466=AXIS2_PLACEMENT_3D('',#16538,#13243,#13244);
#11467=AXIS2_PLACEMENT_3D('',#16547,#13249,#13250);
#11468=AXIS2_PLACEMENT_3D('',#16549,#13251,#13252);
#11469=AXIS2_PLACEMENT_3D('',#16552,#13254,#13255);
#11470=AXIS2_PLACEMENT_3D('',#16553,#13256,#13257);
#11471=AXIS2_PLACEMENT_3D('',#16559,#13261,#13262);
#11472=AXIS2_PLACEMENT_3D('',#16561,#13263,#13264);
#11473=AXIS2_PLACEMENT_3D('',#16564,#13266,#13267);
#11474=AXIS2_PLACEMENT_3D('',#16565,#13268,#13269);
#11475=AXIS2_PLACEMENT_3D('',#16571,#13273,#13274);
#11476=AXIS2_PLACEMENT_3D('',#16573,#13275,#13276);
#11477=AXIS2_PLACEMENT_3D('',#16576,#13278,#13279);
#11478=AXIS2_PLACEMENT_3D('',#16577,#13280,#13281);
#11479=AXIS2_PLACEMENT_3D('',#16583,#13285,#13286);
#11480=AXIS2_PLACEMENT_3D('',#16584,#13287,#13288);
#11481=AXIS2_PLACEMENT_3D('',#16585,#13289,#13290);
#11482=AXIS2_PLACEMENT_3D('',#16586,#13291,#13292);
#11483=AXIS2_PLACEMENT_3D('',#16595,#13297,#13298);
#11484=AXIS2_PLACEMENT_3D('',#16604,#13303,#13304);
#11485=AXIS2_PLACEMENT_3D('',#16613,#13309,#13310);
#11486=AXIS2_PLACEMENT_3D('',#16622,#13315,#13316);
#11487=AXIS2_PLACEMENT_3D('',#16631,#13321,#13322);
#11488=AXIS2_PLACEMENT_3D('',#16632,#13323,#13324);
#11489=AXIS2_PLACEMENT_3D('',#16633,#13325,#13326);
#11490=AXIS2_PLACEMENT_3D('',#16634,#13327,#13328);
#11491=AXIS2_PLACEMENT_3D('',#16635,#13329,#13330);
#11492=AXIS2_PLACEMENT_3D('',#16636,#13331,#13332);
#11493=AXIS2_PLACEMENT_3D('',#16637,#13333,#13334);
#11494=AXIS2_PLACEMENT_3D('',#16638,#13335,#13336);
#11495=AXIS2_PLACEMENT_3D('',#16639,#13337,#13338);
#11496=AXIS2_PLACEMENT_3D('',#16640,#13339,#13340);
#11497=AXIS2_PLACEMENT_3D('',#16641,#13341,#13342);
#11498=AXIS2_PLACEMENT_3D('',#16642,#13343,#13344);
#11499=AXIS2_PLACEMENT_3D('',#16643,#13345,#13346);
#11500=AXIS2_PLACEMENT_3D('',#16644,#13347,#13348);
#11501=AXIS2_PLACEMENT_3D('',#16645,#13349,#13350);
#11502=AXIS2_PLACEMENT_3D('',#16646,#13351,#13352);
#11503=AXIS2_PLACEMENT_3D('',#16647,#13353,#13354);
#11504=AXIS2_PLACEMENT_3D('',#16648,#13355,#13356);
#11505=AXIS2_PLACEMENT_3D('',#16649,#13357,#13358);
#11506=AXIS2_PLACEMENT_3D('',#16650,#13359,#13360);
#11507=AXIS2_PLACEMENT_3D('',#16651,#13361,#13362);
#11508=AXIS2_PLACEMENT_3D('',#16652,#13363,#13364);
#11509=AXIS2_PLACEMENT_3D('',#16653,#13365,#13366);
#11510=AXIS2_PLACEMENT_3D('',#16654,#13367,#13368);
#11511=AXIS2_PLACEMENT_3D('',#16655,#13369,#13370);
#11512=AXIS2_PLACEMENT_3D('',#16656,#13371,#13372);
#11513=AXIS2_PLACEMENT_3D('',#16658,#13373,#13374);
#11514=AXIS2_PLACEMENT_3D('',#16660,#13375,#13376);
#11515=AXIS2_PLACEMENT_3D('',#16661,#13377,#13378);
#11516=AXIS2_PLACEMENT_3D('',#16662,#13379,#13380);
#11517=AXIS2_PLACEMENT_3D('',#16665,#13381,#13382);
#11518=AXIS2_PLACEMENT_3D('',#16666,#13383,#13384);
#11519=AXIS2_PLACEMENT_3D('',#16668,#13385,#13386);
#11520=AXIS2_PLACEMENT_3D('',#16669,#13387,#13388);
#11521=AXIS2_PLACEMENT_3D('',#16670,#13389,#13390);
#11522=AXIS2_PLACEMENT_3D('',#16672,#13391,#13392);
#11523=AXIS2_PLACEMENT_3D('',#16674,#13393,#13394);
#11524=AXIS2_PLACEMENT_3D('',#16675,#13395,#13396);
#11525=AXIS2_PLACEMENT_3D('',#16676,#13397,#13398);
#11526=AXIS2_PLACEMENT_3D('',#16679,#13399,#13400);
#11527=AXIS2_PLACEMENT_3D('',#16680,#13401,#13402);
#11528=AXIS2_PLACEMENT_3D('',#16682,#13403,#13404);
#11529=AXIS2_PLACEMENT_3D('',#16683,#13405,#13406);
#11530=AXIS2_PLACEMENT_3D('',#16684,#13407,#13408);
#11531=AXIS2_PLACEMENT_3D('',#16686,#13410,#13411);
#11532=AXIS2_PLACEMENT_3D('',#16688,#13412,#13413);
#11533=AXIS2_PLACEMENT_3D('',#16691,#13415,#13416);
#11534=AXIS2_PLACEMENT_3D('',#16692,#13417,#13418);
#11535=AXIS2_PLACEMENT_3D('',#16694,#13420,#13421);
#11536=AXIS2_PLACEMENT_3D('',#16695,#13422,#13423);
#11537=AXIS2_PLACEMENT_3D('',#16696,#13424,#13425);
#11538=AXIS2_PLACEMENT_3D('',#16699,#13426,#13427);
#11539=AXIS2_PLACEMENT_3D('',#16703,#13429,#13430);
#11540=AXIS2_PLACEMENT_3D('',#16705,#13432,#13433);
#11541=AXIS2_PLACEMENT_3D('',#16708,#13434,#13435);
#11542=AXIS2_PLACEMENT_3D('',#16712,#13437,#13438);
#11543=AXIS2_PLACEMENT_3D('',#16714,#13440,#13441);
#11544=AXIS2_PLACEMENT_3D('',#16717,#13444,#13445);
#11545=AXIS2_PLACEMENT_3D('',#16719,#13447,#13448);
#11546=AXIS2_PLACEMENT_3D('',#16721,#13450,#13451);
#11547=AXIS2_PLACEMENT_3D('',#16722,#13452,#13453);
#11548=AXIS2_PLACEMENT_3D('',#16723,#13454,#13455);
#11549=AXIS2_PLACEMENT_3D('',#16725,#13456,#13457);
#11550=AXIS2_PLACEMENT_3D('',#16728,#13459,#13460);
#11551=AXIS2_PLACEMENT_3D('',#16729,#13461,#13462);
#11552=AXIS2_PLACEMENT_3D('',#16731,#13463,#13464);
#11553=AXIS2_PLACEMENT_3D('',#16733,#13465,#13466);
#11554=AXIS2_PLACEMENT_3D('',#16734,#13467,#13468);
#11555=AXIS2_PLACEMENT_3D('',#16735,#13469,#13470);
#11556=AXIS2_PLACEMENT_3D('',#16738,#13471,#13472);
#11557=AXIS2_PLACEMENT_3D('',#16739,#13473,#13474);
#11558=AXIS2_PLACEMENT_3D('',#16741,#13475,#13476);
#11559=AXIS2_PLACEMENT_3D('',#16742,#13477,#13478);
#11560=AXIS2_PLACEMENT_3D('',#16743,#13479,#13480);
#11561=AXIS2_PLACEMENT_3D('',#16745,#13481,#13482);
#11562=AXIS2_PLACEMENT_3D('',#16747,#13483,#13484);
#11563=AXIS2_PLACEMENT_3D('',#16748,#13485,#13486);
#11564=AXIS2_PLACEMENT_3D('',#16749,#13487,#13488);
#11565=AXIS2_PLACEMENT_3D('',#16752,#13489,#13490);
#11566=AXIS2_PLACEMENT_3D('',#16753,#13491,#13492);
#11567=AXIS2_PLACEMENT_3D('',#16755,#13493,#13494);
#11568=AXIS2_PLACEMENT_3D('',#16756,#13495,#13496);
#11569=AXIS2_PLACEMENT_3D('',#16757,#13497,#13498);
#11570=AXIS2_PLACEMENT_3D('',#16759,#13500,#13501);
#11571=AXIS2_PLACEMENT_3D('',#16761,#13502,#13503);
#11572=AXIS2_PLACEMENT_3D('',#16764,#13505,#13506);
#11573=AXIS2_PLACEMENT_3D('',#16765,#13507,#13508);
#11574=AXIS2_PLACEMENT_3D('',#16767,#13510,#13511);
#11575=AXIS2_PLACEMENT_3D('',#16768,#13512,#13513);
#11576=AXIS2_PLACEMENT_3D('',#16769,#13514,#13515);
#11577=AXIS2_PLACEMENT_3D('',#16770,#13516,#13517);
#11578=AXIS2_PLACEMENT_3D('',#16771,#13518,#13519);
#11579=AXIS2_PLACEMENT_3D('',#16772,#13520,#13521);
#11580=AXIS2_PLACEMENT_3D('',#16774,#13522,#13523);
#11581=AXIS2_PLACEMENT_3D('',#16776,#13524,#13525);
#11582=AXIS2_PLACEMENT_3D('',#16778,#13526,#13527);
#11583=AXIS2_PLACEMENT_3D('',#16779,#13528,#13529);
#11584=AXIS2_PLACEMENT_3D('',#16780,#13530,#13531);
#11585=AXIS2_PLACEMENT_3D('',#16782,#13532,#13533);
#11586=AXIS2_PLACEMENT_3D('',#16784,#13535,#13536);
#11587=AXIS2_PLACEMENT_3D('',#16786,#13537,#13538);
#11588=AXIS2_PLACEMENT_3D('',#16789,#13540,#13541);
#11589=AXIS2_PLACEMENT_3D('',#16790,#13542,#13543);
#11590=AXIS2_PLACEMENT_3D('',#16792,#13544,#13545);
#11591=AXIS2_PLACEMENT_3D('',#16795,#13547,#13548);
#11592=AXIS2_PLACEMENT_3D('',#16796,#13549,#13550);
#11593=AXIS2_PLACEMENT_3D('',#16798,#13551,#13552);
#11594=AXIS2_PLACEMENT_3D('',#16801,#13554,#13555);
#11595=AXIS2_PLACEMENT_3D('',#16802,#13556,#13557);
#11596=AXIS2_PLACEMENT_3D('',#16804,#13558,#13559);
#11597=AXIS2_PLACEMENT_3D('',#16807,#13561,#13562);
#11598=AXIS2_PLACEMENT_3D('',#16808,#13563,#13564);
#11599=AXIS2_PLACEMENT_3D('',#16810,#13565,#13566);
#11600=AXIS2_PLACEMENT_3D('',#16813,#13568,#13569);
#11601=AXIS2_PLACEMENT_3D('',#16814,#13570,#13571);
#11602=AXIS2_PLACEMENT_3D('',#16816,#13572,#13573);
#11603=AXIS2_PLACEMENT_3D('',#16820,#13575,#13576);
#11604=AXIS2_PLACEMENT_3D('',#16824,#13578,#13579);
#11605=AXIS2_PLACEMENT_3D('',#16828,#13581,#13582);
#11606=AXIS2_PLACEMENT_3D('',#16832,#13584,#13585);
#11607=AXIS2_PLACEMENT_3D('',#16835,#13587,#13588);
#11608=AXIS2_PLACEMENT_3D('',#16836,#13589,#13590);
#11609=AXIS2_PLACEMENT_3D('',#16839,#13591,#13592);
#11610=AXIS2_PLACEMENT_3D('',#16856,#13593,#13594);
#11611=AXIS2_PLACEMENT_3D('',#16871,#13595,#13596);
#11612=AXIS2_PLACEMENT_3D('',#16874,#13597,#13598);
#11613=AXIS2_PLACEMENT_3D('',#16878,#13600,#13601);
#11614=AXIS2_PLACEMENT_3D('',#16880,#13603,#13604);
#11615=AXIS2_PLACEMENT_3D('',#16883,#13605,#13606);
#11616=AXIS2_PLACEMENT_3D('',#16887,#13608,#13609);
#11617=AXIS2_PLACEMENT_3D('',#16889,#13610,#13611);
#11618=AXIS2_PLACEMENT_3D('',#16891,#13613,#13614);
#11619=AXIS2_PLACEMENT_3D('',#16893,#13615,#13616);
#11620=AXIS2_PLACEMENT_3D('',#16897,#13618,#13619);
#11621=AXIS2_PLACEMENT_3D('',#16901,#13621,#13622);
#11622=AXIS2_PLACEMENT_3D('',#16905,#13624,#13625);
#11623=AXIS2_PLACEMENT_3D('',#16909,#13627,#13628);
#11624=AXIS2_PLACEMENT_3D('',#16912,#13630,#13631);
#11625=AXIS2_PLACEMENT_3D('',#16913,#13632,#13633);
#11626=AXIS2_PLACEMENT_3D('',#16919,#13636,#13637);
#11627=AXIS2_PLACEMENT_3D('',#16923,#13639,#13640);
#11628=AXIS2_PLACEMENT_3D('',#16931,#13645,#13646);
#11629=AXIS2_PLACEMENT_3D('',#16945,#13654,#13655);
#11630=AXIS2_PLACEMENT_3D('',#16948,#13658,#13659);
#11631=AXIS2_PLACEMENT_3D('',#16950,#13660,#13661);
#11632=AXIS2_PLACEMENT_3D('',#16955,#13664,#13665);
#11633=AXIS2_PLACEMENT_3D('',#16957,#13667,#13668);
#11634=AXIS2_PLACEMENT_3D('',#16959,#13669,#13670);
#11635=AXIS2_PLACEMENT_3D('',#16961,#13671,#13672);
#11636=AXIS2_PLACEMENT_3D('',#16963,#13674,#13675);
#11637=AXIS2_PLACEMENT_3D('',#16965,#13677,#13678);
#11638=AXIS2_PLACEMENT_3D('',#16972,#13683,#13684);
#11639=AXIS2_PLACEMENT_3D('',#16974,#13686,#13687);
#11640=AXIS2_PLACEMENT_3D('',#16978,#13690,#13691);
#11641=AXIS2_PLACEMENT_3D('',#16979,#13692,#13693);
#11642=AXIS2_PLACEMENT_3D('',#16980,#13694,#13695);
#11643=AXIS2_PLACEMENT_3D('',#16982,#13696,#13697);
#11644=AXIS2_PLACEMENT_3D('',#16984,#13699,#13700);
#11645=AXIS2_PLACEMENT_3D('',#16986,#13702,#13703);
#11646=AXIS2_PLACEMENT_3D('',#16987,#13704,#13705);
#11647=AXIS2_PLACEMENT_3D('',#16988,#13706,#13707);
#11648=AXIS2_PLACEMENT_3D('',#16991,#13710,#13711);
#11649=AXIS2_PLACEMENT_3D('',#16993,#13713,#13714);
#11650=AXIS2_PLACEMENT_3D('',#16995,#13716,#13717);
#11651=AXIS2_PLACEMENT_3D('',#16998,#13718,#13719);
#11652=AXIS2_PLACEMENT_3D('',#17001,#13722,#13723);
#11653=AXIS2_PLACEMENT_3D('',#17016,#13724,#13725);
#11654=AXIS2_PLACEMENT_3D('',#17031,#13726,#13727);
#11655=AXIS2_PLACEMENT_3D('',#17032,#13728,#13729);
#11656=AXIS2_PLACEMENT_3D('',#17035,#13732,#13733);
#11657=AXIS2_PLACEMENT_3D('',#17037,#13735,#13736);
#11658=AXIS2_PLACEMENT_3D('',#17038,#13737,#13738);
#11659=AXIS2_PLACEMENT_3D('',#17040,#13740,#13741);
#11660=AXIS2_PLACEMENT_3D('',#17041,#13742,#13743);
#11661=AXIS2_PLACEMENT_3D('',#17043,#13745,#13746);
#11662=AXIS2_PLACEMENT_3D('',#17044,#13747,#13748);
#11663=AXIS2_PLACEMENT_3D('',#17046,#13750,#13751);
#11664=AXIS2_PLACEMENT_3D('',#17047,#13752,#13753);
#11665=AXIS2_PLACEMENT_3D('',#17053,#13757,#13758);
#11666=AXIS2_PLACEMENT_3D('',#17057,#13761,#13762);
#11667=AXIS2_PLACEMENT_3D('',#17061,#13765,#13766);
#11668=AXIS2_PLACEMENT_3D('',#17063,#13768,#13769);
#11669=AXIS2_PLACEMENT_3D('',#17064,#13770,#13771);
#11670=AXIS2_PLACEMENT_3D('',#17065,#13772,#13773);
#11671=AXIS2_PLACEMENT_3D('',#17066,#13774,#13775);
#11672=AXIS2_PLACEMENT_3D('',#17069,#13776,#13777);
#11673=AXIS2_PLACEMENT_3D('',#17073,#13779,#13780);
#11674=AXIS2_PLACEMENT_3D('',#17075,#13782,#13783);
#11675=AXIS2_PLACEMENT_3D('',#17078,#13784,#13785);
#11676=AXIS2_PLACEMENT_3D('',#17082,#13787,#13788);
#11677=AXIS2_PLACEMENT_3D('',#17084,#13790,#13791);
#11678=AXIS2_PLACEMENT_3D('',#17088,#13793,#13794);
#11679=AXIS2_PLACEMENT_3D('',#17094,#13798,#13799);
#11680=AXIS2_PLACEMENT_3D('',#17095,#13800,#13801);
#11681=AXIS2_PLACEMENT_3D('',#17099,#13803,#13804);
#11682=AXIS2_PLACEMENT_3D('',#17104,#13807,#13808);
#11683=AXIS2_PLACEMENT_3D('',#17106,#13810,#13811);
#11684=AXIS2_PLACEMENT_3D('',#17108,#13813,#13814);
#11685=AXIS2_PLACEMENT_3D('',#17110,#13816,#13817);
#11686=AXIS2_PLACEMENT_3D('',#17111,#13818,#13819);
#11687=AXIS2_PLACEMENT_3D('',#17113,#13821,#13822);
#11688=AXIS2_PLACEMENT_3D('',#17115,#13824,#13825);
#11689=AXIS2_PLACEMENT_3D('',#17116,#13826,#13827);
#11690=AXIS2_PLACEMENT_3D('',#17117,#13828,#13829);
#11691=AXIS2_PLACEMENT_3D('',#17120,#13830,#13831);
#11692=AXIS2_PLACEMENT_3D('',#17124,#13833,#13834);
#11693=AXIS2_PLACEMENT_3D('',#17126,#13836,#13837);
#11694=AXIS2_PLACEMENT_3D('',#17129,#13838,#13839);
#11695=AXIS2_PLACEMENT_3D('',#17133,#13841,#13842);
#11696=AXIS2_PLACEMENT_3D('',#17135,#13844,#13845);
#11697=AXIS2_PLACEMENT_3D('',#17143,#13849,#13850);
#11698=AXIS2_PLACEMENT_3D('',#17150,#13854,#13855);
#11699=AXIS2_PLACEMENT_3D('',#17154,#13858,#13859);
#11700=AXIS2_PLACEMENT_3D('',#17158,#13861,#13862);
#11701=AXIS2_PLACEMENT_3D('',#17171,#13869,#13870);
#11702=AXIS2_PLACEMENT_3D('',#17173,#13872,#13873);
#11703=AXIS2_PLACEMENT_3D('',#17175,#13875,#13876);
#11704=AXIS2_PLACEMENT_3D('',#17177,#13878,#13879);
#11705=AXIS2_PLACEMENT_3D('',#17179,#13881,#13882);
#11706=AXIS2_PLACEMENT_3D('',#17181,#13884,#13885);
#11707=AXIS2_PLACEMENT_3D('',#17182,#13886,#13887);
#11708=AXIS2_PLACEMENT_3D('',#17184,#13889,#13890);
#11709=AXIS2_PLACEMENT_3D('',#17186,#13892,#13893);
#11710=AXIS2_PLACEMENT_3D('',#17188,#13895,#13896);
#11711=AXIS2_PLACEMENT_3D('',#17190,#13898,#13899);
#11712=AXIS2_PLACEMENT_3D('',#17191,#13900,#13901);
#11713=AXIS2_PLACEMENT_3D('',#17192,#13902,#13903);
#11714=AXIS2_PLACEMENT_3D('',#17195,#13904,#13905);
#11715=AXIS2_PLACEMENT_3D('',#17199,#13907,#13908);
#11716=AXIS2_PLACEMENT_3D('',#17201,#13910,#13911);
#11717=AXIS2_PLACEMENT_3D('',#17214,#13917,#13918);
#11718=AXIS2_PLACEMENT_3D('',#17218,#13920,#13921);
#11719=AXIS2_PLACEMENT_3D('',#17222,#13923,#13924);
#11720=AXIS2_PLACEMENT_3D('',#17226,#13926,#13927);
#11721=AXIS2_PLACEMENT_3D('',#17230,#13929,#13930);
#11722=AXIS2_PLACEMENT_3D('',#17234,#13932,#13933);
#11723=AXIS2_PLACEMENT_3D('',#17238,#13935,#13936);
#11724=AXIS2_PLACEMENT_3D('',#17242,#13938,#13939);
#11725=AXIS2_PLACEMENT_3D('',#17246,#13941,#13942);
#11726=AXIS2_PLACEMENT_3D('',#17250,#13944,#13945);
#11727=AXIS2_PLACEMENT_3D('',#17254,#13947,#13948);
#11728=AXIS2_PLACEMENT_3D('',#17272,#13957,#13958);
#11729=AXIS2_PLACEMENT_3D('',#17276,#13960,#13961);
#11730=AXIS2_PLACEMENT_3D('',#17280,#13963,#13964);
#11731=AXIS2_PLACEMENT_3D('',#17284,#13966,#13967);
#11732=AXIS2_PLACEMENT_3D('',#17288,#13969,#13970);
#11733=AXIS2_PLACEMENT_3D('',#17292,#13972,#13973);
#11734=AXIS2_PLACEMENT_3D('',#17296,#13975,#13976);
#11735=AXIS2_PLACEMENT_3D('',#17300,#13978,#13979);
#11736=AXIS2_PLACEMENT_3D('',#17304,#13981,#13982);
#11737=AXIS2_PLACEMENT_3D('',#17308,#13984,#13985);
#11738=AXIS2_PLACEMENT_3D('',#17312,#13987,#13988);
#11739=AXIS2_PLACEMENT_3D('',#17330,#13997,#13998);
#11740=AXIS2_PLACEMENT_3D('',#17334,#14000,#14001);
#11741=AXIS2_PLACEMENT_3D('',#17338,#14003,#14004);
#11742=AXIS2_PLACEMENT_3D('',#17342,#14006,#14007);
#11743=AXIS2_PLACEMENT_3D('',#17346,#14009,#14010);
#11744=AXIS2_PLACEMENT_3D('',#17350,#14012,#14013);
#11745=AXIS2_PLACEMENT_3D('',#17354,#14015,#14016);
#11746=AXIS2_PLACEMENT_3D('',#17358,#14018,#14019);
#11747=AXIS2_PLACEMENT_3D('',#17362,#14021,#14022);
#11748=AXIS2_PLACEMENT_3D('',#17366,#14024,#14025);
#11749=AXIS2_PLACEMENT_3D('',#17370,#14027,#14028);
#11750=AXIS2_PLACEMENT_3D('',#17388,#14037,#14038);
#11751=AXIS2_PLACEMENT_3D('',#17392,#14040,#14041);
#11752=AXIS2_PLACEMENT_3D('',#17396,#14043,#14044);
#11753=AXIS2_PLACEMENT_3D('',#17400,#14046,#14047);
#11754=AXIS2_PLACEMENT_3D('',#17404,#14049,#14050);
#11755=AXIS2_PLACEMENT_3D('',#17408,#14052,#14053);
#11756=AXIS2_PLACEMENT_3D('',#17412,#14055,#14056);
#11757=AXIS2_PLACEMENT_3D('',#17416,#14058,#14059);
#11758=AXIS2_PLACEMENT_3D('',#17420,#14061,#14062);
#11759=AXIS2_PLACEMENT_3D('',#17424,#14064,#14065);
#11760=AXIS2_PLACEMENT_3D('',#17428,#14067,#14068);
#11761=AXIS2_PLACEMENT_3D('',#17438,#14073,#14074);
#11762=AXIS2_PLACEMENT_3D('',#17442,#14076,#14077);
#11763=AXIS2_PLACEMENT_3D('',#17446,#14079,#14080);
#11764=AXIS2_PLACEMENT_3D('',#17449,#14082,#14083);
#11765=AXIS2_PLACEMENT_3D('',#17454,#14085,#14086);
#11766=AXIS2_PLACEMENT_3D('',#17458,#14088,#14089);
#11767=AXIS2_PLACEMENT_3D('',#17462,#14091,#14092);
#11768=AXIS2_PLACEMENT_3D('',#17466,#14094,#14095);
#11769=AXIS2_PLACEMENT_3D('',#17470,#14097,#14098);
#11770=AXIS2_PLACEMENT_3D('',#17474,#14100,#14101);
#11771=AXIS2_PLACEMENT_3D('',#17478,#14104,#14105);
#11772=AXIS2_PLACEMENT_3D('',#17483,#14107,#14108);
#11773=AXIS2_PLACEMENT_3D('',#17487,#14110,#14111);
#11774=AXIS2_PLACEMENT_3D('',#17491,#14113,#14114);
#11775=AXIS2_PLACEMENT_3D('',#17494,#14116,#14117);
#11776=AXIS2_PLACEMENT_3D('',#17499,#14119,#14120);
#11777=AXIS2_PLACEMENT_3D('',#17503,#14122,#14123);
#11778=AXIS2_PLACEMENT_3D('',#17507,#14125,#14126);
#11779=AXIS2_PLACEMENT_3D('',#17510,#14128,#14129);
#11780=AXIS2_PLACEMENT_3D('',#17515,#14131,#14132);
#11781=AXIS2_PLACEMENT_3D('',#17519,#14134,#14135);
#11782=AXIS2_PLACEMENT_3D('',#17523,#14137,#14138);
#11783=AXIS2_PLACEMENT_3D('',#17526,#14140,#14141);
#11784=AXIS2_PLACEMENT_3D('',#17527,#14142,#14143);
#11785=AXIS2_PLACEMENT_3D('',#17538,#14148,#14149);
#11786=AXIS2_PLACEMENT_3D('',#17542,#14151,#14152);
#11787=AXIS2_PLACEMENT_3D('',#17546,#14154,#14155);
#11788=AXIS2_PLACEMENT_3D('',#17550,#14157,#14158);
#11789=AXIS2_PLACEMENT_3D('',#17554,#14160,#14161);
#11790=AXIS2_PLACEMENT_3D('',#17558,#14163,#14164);
#11791=AXIS2_PLACEMENT_3D('',#17562,#14166,#14167);
#11792=AXIS2_PLACEMENT_3D('',#17566,#14169,#14170);
#11793=AXIS2_PLACEMENT_3D('',#17570,#14172,#14173);
#11794=AXIS2_PLACEMENT_3D('',#17574,#14175,#14176);
#11795=AXIS2_PLACEMENT_3D('',#17578,#14178,#14179);
#11796=AXIS2_PLACEMENT_3D('',#17596,#14188,#14189);
#11797=AXIS2_PLACEMENT_3D('',#17600,#14191,#14192);
#11798=AXIS2_PLACEMENT_3D('',#17604,#14194,#14195);
#11799=AXIS2_PLACEMENT_3D('',#17608,#14197,#14198);
#11800=AXIS2_PLACEMENT_3D('',#17612,#14200,#14201);
#11801=AXIS2_PLACEMENT_3D('',#17616,#14203,#14204);
#11802=AXIS2_PLACEMENT_3D('',#17620,#14206,#14207);
#11803=AXIS2_PLACEMENT_3D('',#17624,#14209,#14210);
#11804=AXIS2_PLACEMENT_3D('',#17628,#14212,#14213);
#11805=AXIS2_PLACEMENT_3D('',#17632,#14215,#14216);
#11806=AXIS2_PLACEMENT_3D('',#17636,#14218,#14219);
#11807=AXIS2_PLACEMENT_3D('',#17654,#14228,#14229);
#11808=AXIS2_PLACEMENT_3D('',#17658,#14231,#14232);
#11809=AXIS2_PLACEMENT_3D('',#17662,#14234,#14235);
#11810=AXIS2_PLACEMENT_3D('',#17666,#14237,#14238);
#11811=AXIS2_PLACEMENT_3D('',#17670,#14240,#14241);
#11812=AXIS2_PLACEMENT_3D('',#17674,#14243,#14244);
#11813=AXIS2_PLACEMENT_3D('',#17678,#14246,#14247);
#11814=AXIS2_PLACEMENT_3D('',#17682,#14249,#14250);
#11815=AXIS2_PLACEMENT_3D('',#17686,#14252,#14253);
#11816=AXIS2_PLACEMENT_3D('',#17690,#14255,#14256);
#11817=AXIS2_PLACEMENT_3D('',#17694,#14258,#14259);
#11818=AXIS2_PLACEMENT_3D('',#17712,#14268,#14269);
#11819=AXIS2_PLACEMENT_3D('',#17716,#14271,#14272);
#11820=AXIS2_PLACEMENT_3D('',#17720,#14274,#14275);
#11821=AXIS2_PLACEMENT_3D('',#17724,#14277,#14278);
#11822=AXIS2_PLACEMENT_3D('',#17728,#14280,#14281);
#11823=AXIS2_PLACEMENT_3D('',#17732,#14283,#14284);
#11824=AXIS2_PLACEMENT_3D('',#17736,#14286,#14287);
#11825=AXIS2_PLACEMENT_3D('',#17740,#14289,#14290);
#11826=AXIS2_PLACEMENT_3D('',#17744,#14292,#14293);
#11827=AXIS2_PLACEMENT_3D('',#17748,#14295,#14296);
#11828=AXIS2_PLACEMENT_3D('',#17752,#14298,#14299);
#11829=AXIS2_PLACEMENT_3D('',#17762,#14304,#14305);
#11830=AXIS2_PLACEMENT_3D('',#17766,#14307,#14308);
#11831=AXIS2_PLACEMENT_3D('',#17770,#14310,#14311);
#11832=AXIS2_PLACEMENT_3D('',#17774,#14313,#14314);
#11833=AXIS2_PLACEMENT_3D('',#17778,#14316,#14317);
#11834=AXIS2_PLACEMENT_3D('',#17782,#14319,#14320);
#11835=AXIS2_PLACEMENT_3D('',#17786,#14322,#14323);
#11836=AXIS2_PLACEMENT_3D('',#17790,#14325,#14326);
#11837=AXIS2_PLACEMENT_3D('',#17794,#14328,#14329);
#11838=AXIS2_PLACEMENT_3D('',#17798,#14331,#14332);
#11839=AXIS2_PLACEMENT_3D('',#17802,#14334,#14335);
#11840=AXIS2_PLACEMENT_3D('',#17806,#14337,#14338);
#11841=AXIS2_PLACEMENT_3D('',#17810,#14340,#14341);
#11842=AXIS2_PLACEMENT_3D('',#17814,#14343,#14344);
#11843=AXIS2_PLACEMENT_3D('',#17818,#14346,#14347);
#11844=AXIS2_PLACEMENT_3D('',#17822,#14349,#14350);
#11845=AXIS2_PLACEMENT_3D('',#17826,#14352,#14353);
#11846=AXIS2_PLACEMENT_3D('',#17830,#14355,#14356);
#11847=AXIS2_PLACEMENT_3D('',#17835,#14359,#14360);
#11848=AXIS2_PLACEMENT_3D('',#17839,#14362,#14363);
#11849=AXIS2_PLACEMENT_3D('',#17843,#14365,#14366);
#11850=AXIS2_PLACEMENT_3D('',#17847,#14368,#14369);
#11851=AXIS2_PLACEMENT_3D('',#17851,#14371,#14372);
#11852=AXIS2_PLACEMENT_3D('',#17853,#14374,#14375);
#11853=AXIS2_PLACEMENT_3D('',#17856,#14378,#14379);
#11854=AXIS2_PLACEMENT_3D('',#17858,#14381,#14382);
#11855=AXIS2_PLACEMENT_3D('',#17860,#14384,#14385);
#11856=AXIS2_PLACEMENT_3D('',#17862,#14387,#14388);
#11857=AXIS2_PLACEMENT_3D('',#17864,#14390,#14391);
#11858=AXIS2_PLACEMENT_3D('',#17866,#14393,#14394);
#11859=AXIS2_PLACEMENT_3D('',#17868,#14396,#14397);
#11860=AXIS2_PLACEMENT_3D('',#17870,#14399,#14400);
#11861=AXIS2_PLACEMENT_3D('',#17872,#14402,#14403);
#11862=AXIS2_PLACEMENT_3D('',#17874,#14405,#14406);
#11863=AXIS2_PLACEMENT_3D('',#17876,#14408,#14409);
#11864=AXIS2_PLACEMENT_3D('',#17878,#14411,#14412);
#11865=AXIS2_PLACEMENT_3D('',#17880,#14414,#14415);
#11866=AXIS2_PLACEMENT_3D('',#17882,#14417,#14418);
#11867=AXIS2_PLACEMENT_3D('',#17884,#14420,#14421);
#11868=AXIS2_PLACEMENT_3D('',#17886,#14423,#14424);
#11869=AXIS2_PLACEMENT_3D('',#17888,#14426,#14427);
#11870=AXIS2_PLACEMENT_3D('',#17890,#14429,#14430);
#11871=AXIS2_PLACEMENT_3D('',#17892,#14432,#14433);
#11872=AXIS2_PLACEMENT_3D('',#17894,#14435,#14436);
#11873=AXIS2_PLACEMENT_3D('',#17896,#14438,#14439);
#11874=AXIS2_PLACEMENT_3D('',#17898,#14441,#14442);
#11875=AXIS2_PLACEMENT_3D('',#17900,#14444,#14445);
#11876=AXIS2_PLACEMENT_3D('',#17902,#14447,#14448);
#11877=AXIS2_PLACEMENT_3D('',#17904,#14450,#14451);
#11878=AXIS2_PLACEMENT_3D('',#17906,#14453,#14454);
#11879=AXIS2_PLACEMENT_3D('',#17908,#14456,#14457);
#11880=AXIS2_PLACEMENT_3D('',#17910,#14459,#14460);
#11881=AXIS2_PLACEMENT_3D('',#17912,#14462,#14463);
#11882=AXIS2_PLACEMENT_3D('',#17914,#14465,#14466);
#11883=AXIS2_PLACEMENT_3D('',#17916,#14468,#14469);
#11884=AXIS2_PLACEMENT_3D('',#17918,#14471,#14472);
#11885=AXIS2_PLACEMENT_3D('',#17920,#14474,#14475);
#11886=AXIS2_PLACEMENT_3D('',#17922,#14477,#14478);
#11887=AXIS2_PLACEMENT_3D('',#17924,#14480,#14481);
#11888=AXIS2_PLACEMENT_3D('',#17926,#14483,#14484);
#11889=AXIS2_PLACEMENT_3D('',#17928,#14486,#14487);
#11890=AXIS2_PLACEMENT_3D('',#17930,#14489,#14490);
#11891=AXIS2_PLACEMENT_3D('',#17932,#14492,#14493);
#11892=AXIS2_PLACEMENT_3D('',#17934,#14495,#14496);
#11893=AXIS2_PLACEMENT_3D('',#17936,#14498,#14499);
#11894=AXIS2_PLACEMENT_3D('',#17938,#14501,#14502);
#11895=AXIS2_PLACEMENT_3D('',#17940,#14504,#14505);
#11896=AXIS2_PLACEMENT_3D('',#17942,#14507,#14508);
#11897=AXIS2_PLACEMENT_3D('',#17944,#14510,#14511);
#11898=AXIS2_PLACEMENT_3D('',#17946,#14513,#14514);
#11899=AXIS2_PLACEMENT_3D('',#17948,#14516,#14517);
#11900=AXIS2_PLACEMENT_3D('',#17950,#14519,#14520);
#11901=AXIS2_PLACEMENT_3D('',#17952,#14522,#14523);
#11902=AXIS2_PLACEMENT_3D('',#17954,#14525,#14526);
#11903=AXIS2_PLACEMENT_3D('',#17956,#14528,#14529);
#11904=AXIS2_PLACEMENT_3D('',#17958,#14531,#14532);
#11905=AXIS2_PLACEMENT_3D('',#17960,#14534,#14535);
#11906=AXIS2_PLACEMENT_3D('',#17962,#14537,#14538);
#11907=AXIS2_PLACEMENT_3D('',#17964,#14540,#14541);
#11908=AXIS2_PLACEMENT_3D('',#17966,#14543,#14544);
#11909=AXIS2_PLACEMENT_3D('',#17968,#14546,#14547);
#11910=AXIS2_PLACEMENT_3D('',#17970,#14549,#14550);
#11911=AXIS2_PLACEMENT_3D('',#17972,#14552,#14553);
#11912=AXIS2_PLACEMENT_3D('',#17974,#14555,#14556);
#11913=AXIS2_PLACEMENT_3D('',#17976,#14558,#14559);
#11914=AXIS2_PLACEMENT_3D('',#17978,#14561,#14562);
#11915=AXIS2_PLACEMENT_3D('',#17980,#14564,#14565);
#11916=AXIS2_PLACEMENT_3D('',#17982,#14567,#14568);
#11917=AXIS2_PLACEMENT_3D('',#17984,#14570,#14571);
#11918=AXIS2_PLACEMENT_3D('',#17986,#14573,#14574);
#11919=AXIS2_PLACEMENT_3D('',#17988,#14576,#14577);
#11920=AXIS2_PLACEMENT_3D('',#17990,#14579,#14580);
#11921=AXIS2_PLACEMENT_3D('',#17992,#14582,#14583);
#11922=AXIS2_PLACEMENT_3D('',#17994,#14585,#14586);
#11923=AXIS2_PLACEMENT_3D('',#17996,#14588,#14589);
#11924=AXIS2_PLACEMENT_3D('',#17998,#14591,#14592);
#11925=AXIS2_PLACEMENT_3D('',#18000,#14594,#14595);
#11926=AXIS2_PLACEMENT_3D('',#18002,#14597,#14598);
#11927=AXIS2_PLACEMENT_3D('',#18004,#14600,#14601);
#11928=AXIS2_PLACEMENT_3D('',#18006,#14603,#14604);
#11929=AXIS2_PLACEMENT_3D('',#18008,#14606,#14607);
#11930=AXIS2_PLACEMENT_3D('',#18010,#14609,#14610);
#11931=AXIS2_PLACEMENT_3D('',#18012,#14612,#14613);
#11932=AXIS2_PLACEMENT_3D('',#18014,#14615,#14616);
#11933=AXIS2_PLACEMENT_3D('',#18016,#14618,#14619);
#11934=AXIS2_PLACEMENT_3D('',#18018,#14621,#14622);
#11935=AXIS2_PLACEMENT_3D('',#18020,#14624,#14625);
#11936=AXIS2_PLACEMENT_3D('',#18022,#14627,#14628);
#11937=AXIS2_PLACEMENT_3D('',#18024,#14630,#14631);
#11938=AXIS2_PLACEMENT_3D('',#18026,#14633,#14634);
#11939=AXIS2_PLACEMENT_3D('',#18028,#14636,#14637);
#11940=AXIS2_PLACEMENT_3D('',#18030,#14639,#14640);
#11941=AXIS2_PLACEMENT_3D('',#18032,#14642,#14643);
#11942=AXIS2_PLACEMENT_3D('',#18034,#14645,#14646);
#11943=AXIS2_PLACEMENT_3D('',#18036,#14648,#14649);
#11944=AXIS2_PLACEMENT_3D('',#18038,#14651,#14652);
#11945=AXIS2_PLACEMENT_3D('',#18040,#14654,#14655);
#11946=AXIS2_PLACEMENT_3D('',#18042,#14657,#14658);
#11947=AXIS2_PLACEMENT_3D('',#18044,#14660,#14661);
#11948=AXIS2_PLACEMENT_3D('',#18046,#14663,#14664);
#11949=AXIS2_PLACEMENT_3D('',#18048,#14666,#14667);
#11950=AXIS2_PLACEMENT_3D('',#18050,#14669,#14670);
#11951=AXIS2_PLACEMENT_3D('',#18052,#14672,#14673);
#11952=AXIS2_PLACEMENT_3D('',#18054,#14675,#14676);
#11953=AXIS2_PLACEMENT_3D('',#18056,#14678,#14679);
#11954=AXIS2_PLACEMENT_3D('',#18058,#14681,#14682);
#11955=AXIS2_PLACEMENT_3D('',#18060,#14684,#14685);
#11956=AXIS2_PLACEMENT_3D('',#18062,#14687,#14688);
#11957=AXIS2_PLACEMENT_3D('',#18064,#14690,#14691);
#11958=AXIS2_PLACEMENT_3D('',#18066,#14693,#14694);
#11959=AXIS2_PLACEMENT_3D('',#18068,#14696,#14697);
#11960=AXIS2_PLACEMENT_3D('',#18070,#14699,#14700);
#11961=AXIS2_PLACEMENT_3D('',#18072,#14702,#14703);
#11962=AXIS2_PLACEMENT_3D('',#18074,#14705,#14706);
#11963=AXIS2_PLACEMENT_3D('',#18076,#14708,#14709);
#11964=AXIS2_PLACEMENT_3D('',#18078,#14711,#14712);
#11965=AXIS2_PLACEMENT_3D('',#18080,#14714,#14715);
#11966=AXIS2_PLACEMENT_3D('',#18082,#14717,#14718);
#11967=AXIS2_PLACEMENT_3D('',#18084,#14720,#14721);
#11968=AXIS2_PLACEMENT_3D('',#18085,#14722,#14723);
#11969=AXIS2_PLACEMENT_3D('',#18088,#14726,#14727);
#11970=AXIS2_PLACEMENT_3D('',#18090,#14729,#14730);
#11971=AXIS2_PLACEMENT_3D('',#18092,#14732,#14733);
#11972=AXIS2_PLACEMENT_3D('',#18094,#14735,#14736);
#11973=AXIS2_PLACEMENT_3D('',#18096,#14738,#14739);
#11974=AXIS2_PLACEMENT_3D('',#18098,#14741,#14742);
#11975=AXIS2_PLACEMENT_3D('',#18100,#14744,#14745);
#11976=AXIS2_PLACEMENT_3D('',#18101,#14746,#14747);
#11977=AXIS2_PLACEMENT_3D('',#18104,#14750,#14751);
#11978=AXIS2_PLACEMENT_3D('',#18106,#14753,#14754);
#11979=AXIS2_PLACEMENT_3D('',#18108,#14756,#14757);
#11980=AXIS2_PLACEMENT_3D('',#18109,#14758,#14759);
#11981=AXIS2_PLACEMENT_3D('',#18111,#14761,#14762);
#11982=AXIS2_PLACEMENT_3D('',#18113,#14764,#14765);
#11983=AXIS2_PLACEMENT_3D('',#18115,#14767,#14768);
#11984=AXIS2_PLACEMENT_3D('',#18117,#14770,#14771);
#11985=AXIS2_PLACEMENT_3D('',#18119,#14773,#14774);
#11986=AXIS2_PLACEMENT_3D('',#18121,#14776,#14777);
#11987=AXIS2_PLACEMENT_3D('',#18123,#14779,#14780);
#11988=AXIS2_PLACEMENT_3D('',#18125,#14782,#14783);
#11989=AXIS2_PLACEMENT_3D('',#18127,#14785,#14786);
#11990=AXIS2_PLACEMENT_3D('',#18129,#14788,#14789);
#11991=AXIS2_PLACEMENT_3D('',#18130,#14790,#14791);
#11992=AXIS2_PLACEMENT_3D('',#18133,#14794,#14795);
#11993=AXIS2_PLACEMENT_3D('',#18135,#14797,#14798);
#11994=AXIS2_PLACEMENT_3D('',#18137,#14800,#14801);
#11995=AXIS2_PLACEMENT_3D('',#18139,#14803,#14804);
#11996=AXIS2_PLACEMENT_3D('',#18141,#14806,#14807);
#11997=AXIS2_PLACEMENT_3D('',#18143,#14809,#14810);
#11998=AXIS2_PLACEMENT_3D('',#18145,#14812,#14813);
#11999=AXIS2_PLACEMENT_3D('',#18146,#14814,#14815);
#12000=AXIS2_PLACEMENT_3D('',#18149,#14818,#14819);
#12001=AXIS2_PLACEMENT_3D('',#18151,#14821,#14822);
#12002=AXIS2_PLACEMENT_3D('',#18153,#14824,#14825);
#12003=AXIS2_PLACEMENT_3D('',#18155,#14827,#14828);
#12004=AXIS2_PLACEMENT_3D('',#18157,#14830,#14831);
#12005=AXIS2_PLACEMENT_3D('',#18159,#14833,#14834);
#12006=AXIS2_PLACEMENT_3D('',#18161,#14836,#14837);
#12007=AXIS2_PLACEMENT_3D('',#18162,#14838,#14839);
#12008=AXIS2_PLACEMENT_3D('',#18165,#14842,#14843);
#12009=AXIS2_PLACEMENT_3D('',#18167,#14845,#14846);
#12010=AXIS2_PLACEMENT_3D('',#18169,#14848,#14849);
#12011=AXIS2_PLACEMENT_3D('',#18171,#14851,#14852);
#12012=AXIS2_PLACEMENT_3D('',#18173,#14854,#14855);
#12013=AXIS2_PLACEMENT_3D('',#18175,#14857,#14858);
#12014=AXIS2_PLACEMENT_3D('',#18177,#14860,#14861);
#12015=AXIS2_PLACEMENT_3D('',#18178,#14862,#14863);
#12016=AXIS2_PLACEMENT_3D('',#18179,#14864,#14865);
#12017=AXIS2_PLACEMENT_3D('',#18181,#14866,#14867);
#12018=AXIS2_PLACEMENT_3D('',#18184,#14869,#14870);
#12019=AXIS2_PLACEMENT_3D('',#18185,#14871,#14872);
#12020=AXIS2_PLACEMENT_3D('',#18187,#14873,#14874);
#12021=AXIS2_PLACEMENT_3D('',#18190,#14876,#14877);
#12022=AXIS2_PLACEMENT_3D('',#18191,#14878,#14879);
#12023=AXIS2_PLACEMENT_3D('',#18201,#14884,#14885);
#12024=AXIS2_PLACEMENT_3D('',#18202,#14886,#14887);
#12025=AXIS2_PLACEMENT_3D('',#18212,#14892,#14893);
#12026=AXIS2_PLACEMENT_3D('',#18213,#14894,#14895);
#12027=AXIS2_PLACEMENT_3D('',#18222,#14899,#14900);
#12028=AXIS2_PLACEMENT_3D('',#18224,#14902,#14903);
#12029=AXIS2_PLACEMENT_3D('',#18235,#14910,#14911);
#12030=AXIS2_PLACEMENT_3D('',#18237,#14912,#14913);
#12031=AXIS2_PLACEMENT_3D('',#18244,#14917,#14918);
#12032=AXIS2_PLACEMENT_3D('',#18245,#14919,#14920);
#12033=AXIS2_PLACEMENT_3D('',#18262,#14929,#14930);
#12034=AXIS2_PLACEMENT_3D('',#18271,#14934,#14935);
#12035=AXIS2_PLACEMENT_3D('',#18273,#14937,#14938);
#12036=AXIS2_PLACEMENT_3D('',#18284,#14945,#14946);
#12037=AXIS2_PLACEMENT_3D('',#18288,#14948,#14949);
#12038=AXIS2_PLACEMENT_3D('',#18290,#14950,#14951);
#12039=AXIS2_PLACEMENT_3D('',#18294,#14954,#14955);
#12040=AXIS2_PLACEMENT_3D('',#18311,#14964,#14965);
#12041=AXIS2_PLACEMENT_3D('',#18312,#14966,#14967);
#12042=AXIS2_PLACEMENT_3D('',#18314,#14969,#14970);
#12043=AXIS2_PLACEMENT_3D('',#18315,#14971,#14972);
#12044=AXIS2_PLACEMENT_3D('',#18317,#14974,#14975);
#12045=AXIS2_PLACEMENT_3D('',#18320,#14976,#14977);
#12046=AXIS2_PLACEMENT_3D('',#18324,#14979,#14980);
#12047=AXIS2_PLACEMENT_3D('',#18326,#14982,#14983);
#12048=AXIS2_PLACEMENT_3D('',#18327,#14984,#14985);
#12049=AXIS2_PLACEMENT_3D('',#18328,#14986,#14987);
#12050=AXIS2_PLACEMENT_3D('',#18330,#14989,#14990);
#12051=AXIS2_PLACEMENT_3D('',#18331,#14991,#14992);
#12052=AXIS2_PLACEMENT_3D('',#18337,#14995,#14996);
#12053=AXIS2_PLACEMENT_3D('',#18340,#14998,#14999);
#12054=AXIS2_PLACEMENT_3D('',#18341,#15000,#15001);
#12055=AXIS2_PLACEMENT_3D('',#18344,#15004,#15005);
#12056=AXIS2_PLACEMENT_3D('',#18346,#15007,#15008);
#12057=AXIS2_PLACEMENT_3D('',#18348,#15010,#15011);
#12058=AXIS2_PLACEMENT_3D('',#18349,#15012,#15013);
#12059=AXIS2_PLACEMENT_3D('',#18350,#15014,#15015);
#12060=AXIS2_PLACEMENT_3D('',#18351,#15016,#15017);
#12061=AXIS2_PLACEMENT_3D('',#18352,#15018,#15019);
#12062=AXIS2_PLACEMENT_3D('',#18353,#15020,#15021);
#12063=AXIS2_PLACEMENT_3D('',#18354,#15022,#15023);
#12064=AXIS2_PLACEMENT_3D('',#18355,#15024,#15025);
#12065=AXIS2_PLACEMENT_3D('',#18356,#15026,#15027);
#12066=AXIS2_PLACEMENT_3D('',#18358,#15028,#15029);
#12067=AXIS2_PLACEMENT_3D('',#18360,#15031,#15032);
#12068=AXIS2_PLACEMENT_3D('',#18363,#15034,#15035);
#12069=AXIS2_PLACEMENT_3D('',#18364,#15036,#15037);
#12070=AXIS2_PLACEMENT_3D('',#18365,#15038,#15039);
#12071=AXIS2_PLACEMENT_3D('',#18367,#15041,#15042);
#12072=AXIS2_PLACEMENT_3D('',#18368,#15043,#15044);
#12073=AXIS2_PLACEMENT_3D('',#18370,#15045,#15046);
#12074=AXIS2_PLACEMENT_3D('',#18372,#15048,#15049);
#12075=AXIS2_PLACEMENT_3D('',#18375,#15051,#15052);
#12076=AXIS2_PLACEMENT_3D('',#18376,#15053,#15054);
#12077=AXIS2_PLACEMENT_3D('',#18377,#15055,#15056);
#12078=AXIS2_PLACEMENT_3D('',#18379,#15058,#15059);
#12079=AXIS2_PLACEMENT_3D('',#18380,#15060,#15061);
#12080=AXIS2_PLACEMENT_3D('',#18381,#15062,#15063);
#12081=AXIS2_PLACEMENT_3D('',#18382,#15064,#15065);
#12082=AXIS2_PLACEMENT_3D('',#18383,#15066,#15067);
#12083=AXIS2_PLACEMENT_3D('',#18384,#15068,#15069);
#12084=AXIS2_PLACEMENT_3D('',#18385,#15070,#15071);
#12085=AXIS2_PLACEMENT_3D('',#18386,#15072,#15073);
#12086=AXIS2_PLACEMENT_3D('',#18388,#15074,#15075);
#12087=AXIS2_PLACEMENT_3D('',#18391,#15077,#15078);
#12088=AXIS2_PLACEMENT_3D('',#18392,#15079,#15080);
#12089=AXIS2_PLACEMENT_3D('',#18394,#15081,#15082);
#12090=AXIS2_PLACEMENT_3D('',#18397,#15084,#15085);
#12091=AXIS2_PLACEMENT_3D('',#18398,#15086,#15087);
#12092=AXIS2_PLACEMENT_3D('',#18403,#15089,#15090);
#12093=AXIS2_PLACEMENT_3D('',#18407,#15092,#15093);
#12094=AXIS2_PLACEMENT_3D('',#18411,#15096,#15097);
#12095=AXIS2_PLACEMENT_3D('',#18428,#15106,#15107);
#12096=AXIS2_PLACEMENT_3D('',#18434,#15111,#15112);
#12097=AXIS2_PLACEMENT_3D('',#18440,#15116,#15117);
#12098=AXIS2_PLACEMENT_3D('',#18449,#15123,#15124);
#12099=AXIS2_PLACEMENT_3D('',#18458,#15130,#15131);
#12100=AXIS2_PLACEMENT_3D('',#18464,#15135,#15136);
#12101=AXIS2_PLACEMENT_3D('',#18465,#15137,#15138);
#12102=AXIS2_PLACEMENT_3D('',#18471,#15142,#15143);
#12103=AXIS2_PLACEMENT_3D('',#18472,#15144,#15145);
#12104=AXIS2_PLACEMENT_3D('',#18474,#15147,#15148);
#12105=AXIS2_PLACEMENT_3D('',#18476,#15150,#15151);
#12106=AXIS2_PLACEMENT_3D('',#18477,#15152,#15153);
#12107=AXIS2_PLACEMENT_3D('',#18479,#15155,#15156);
#12108=AXIS2_PLACEMENT_3D('',#18481,#15158,#15159);
#12109=AXIS2_PLACEMENT_3D('',#18482,#15160,#15161);
#12110=AXIS2_PLACEMENT_3D('',#18483,#15162,#15163);
#12111=AXIS2_PLACEMENT_3D('',#18484,#15164,#15165);
#12112=AXIS2_PLACEMENT_3D('',#18485,#15166,#15167);
#12113=AXIS2_PLACEMENT_3D('',#18486,#15168,#15169);
#12114=AXIS2_PLACEMENT_3D('',#18491,#15171,#15172);
#12115=AXIS2_PLACEMENT_3D('',#18495,#15174,#15175);
#12116=AXIS2_PLACEMENT_3D('',#18499,#15177,#15178);
#12117=AXIS2_PLACEMENT_3D('',#18502,#15180,#15181);
#12118=AXIS2_PLACEMENT_3D('',#18511,#15186,#15187);
#12119=AXIS2_PLACEMENT_3D('',#18516,#15189,#15190);
#12120=AXIS2_PLACEMENT_3D('',#18520,#15192,#15193);
#12121=AXIS2_PLACEMENT_3D('',#18524,#15195,#15196);
#12122=AXIS2_PLACEMENT_3D('',#18527,#15198,#15199);
#12123=AXIS2_PLACEMENT_3D('',#18536,#15204,#15205);
#12124=AXIS2_PLACEMENT_3D('',#18539,#15208,#15209);
#12125=AXIS2_PLACEMENT_3D('',#18542,#15212,#15213);
#12126=AXIS2_PLACEMENT_3D('',#18545,#15216,#15217);
#12127=AXIS2_PLACEMENT_3D('',#18548,#15220,#15221);
#12128=AXIS2_PLACEMENT_3D('',#18551,#15224,#15225);
#12129=AXIS2_PLACEMENT_3D('',#18553,#15227,#15228);
#12130=AXIS2_PLACEMENT_3D('',#18555,#15230,#15231);
#12131=AXIS2_PLACEMENT_3D('',#18556,#15232,#15233);
#12132=AXIS2_PLACEMENT_3D('',#18557,#15234,#15235);
#12133=AXIS2_PLACEMENT_3D('',#18558,#15236,#15237);
#12134=AXIS2_PLACEMENT_3D('',#18559,#15238,#15239);
#12135=AXIS2_PLACEMENT_3D('',#18560,#15240,#15241);
#12136=AXIS2_PLACEMENT_3D('',#18561,#15242,#15243);
#12137=AXIS2_PLACEMENT_3D('',#18563,#15244,#15245);
#12138=AXIS2_PLACEMENT_3D('',#18566,#15247,#15248);
#12139=AXIS2_PLACEMENT_3D('',#18567,#15249,#15250);
#12140=AXIS2_PLACEMENT_3D('',#18570,#15251,#15252);
#12141=AXIS2_PLACEMENT_3D('',#18571,#15253,#15254);
#12142=AXIS2_PLACEMENT_3D('',#18574,#15256,#15257);
#12143=AXIS2_PLACEMENT_3D('',#18575,#15258,#15259);
#12144=AXIS2_PLACEMENT_3D('',#18578,#15261,#15262);
#12145=AXIS2_PLACEMENT_3D('',#18579,#15263,#15264);
#12146=AXIS2_PLACEMENT_3D('',#18581,#15265,#15266);
#12147=AXIS2_PLACEMENT_3D('',#18584,#15268,#15269);
#12148=AXIS2_PLACEMENT_3D('',#18585,#15270,#15271);
#12149=AXIS2_PLACEMENT_3D('',#18587,#15272,#15273);
#12150=AXIS2_PLACEMENT_3D('',#18590,#15275,#15276);
#12151=AXIS2_PLACEMENT_3D('',#18591,#15277,#15278);
#12152=AXIS2_PLACEMENT_3D('',#18593,#15279,#15280);
#12153=AXIS2_PLACEMENT_3D('',#18596,#15282,#15283);
#12154=AXIS2_PLACEMENT_3D('',#18597,#15284,#15285);
#12155=AXIS2_PLACEMENT_3D('',#18599,#15286,#15287);
#12156=AXIS2_PLACEMENT_3D('',#18602,#15289,#15290);
#12157=AXIS2_PLACEMENT_3D('',#18603,#15291,#15292);
#12158=AXIS2_PLACEMENT_3D('',#18604,#15293,#15294);
#12159=AXIS2_PLACEMENT_3D('',#18605,#15295,#15296);
#12160=AXIS2_PLACEMENT_3D('',#18606,#15297,#15298);
#12161=AXIS2_PLACEMENT_3D('',#18607,#15299,#15300);
#12162=AXIS2_PLACEMENT_3D('',#18608,#15301,#15302);
#12163=AXIS2_PLACEMENT_3D('',#18609,#15303,#15304);
#12164=AXIS2_PLACEMENT_3D('',#18610,#15305,#15306);
#12165=AXIS2_PLACEMENT_3D('',#18613,#15307,#15308);
#12166=AXIS2_PLACEMENT_3D('',#18614,#15309,#15310);
#12167=AXIS2_PLACEMENT_3D('',#18617,#15311,#15312);
#12168=AXIS2_PLACEMENT_3D('',#18618,#15313,#15314);
#12169=AXIS2_PLACEMENT_3D('',#18621,#15315,#15316);
#12170=AXIS2_PLACEMENT_3D('',#18622,#15317,#15318);
#12171=AXIS2_PLACEMENT_3D('',#18625,#15319,#15320);
#12172=AXIS2_PLACEMENT_3D('',#18626,#15321,#15322);
#12173=AXIS2_PLACEMENT_3D('',#18629,#15323,#15324);
#12174=AXIS2_PLACEMENT_3D('',#18630,#15325,#15326);
#12175=AXIS2_PLACEMENT_3D('',#18633,#15327,#15328);
#12176=AXIS2_PLACEMENT_3D('',#18634,#15329,#15330);
#12177=AXIS2_PLACEMENT_3D('',#18637,#15331,#15332);
#12178=AXIS2_PLACEMENT_3D('',#18638,#15333,#15334);
#12179=AXIS2_PLACEMENT_3D('',#18640,#15335,#15336);
#12180=AXIS2_PLACEMENT_3D('',#18642,#15337,#15338);
#12181=AXIS2_PLACEMENT_3D('',#18643,#15339,#15340);
#12182=AXIS2_PLACEMENT_3D('',#18644,#15341,#15342);
#12183=AXIS2_PLACEMENT_3D('',#18646,#15343,#15344);
#12184=AXIS2_PLACEMENT_3D('',#18648,#15346,#15347);
#12185=AXIS2_PLACEMENT_3D('',#18650,#15348,#15349);
#12186=AXIS2_PLACEMENT_3D('',#18651,#15350,#15351);
#12187=AXIS2_PLACEMENT_3D('',#18652,#15352,#15353);
#12188=AXIS2_PLACEMENT_3D('',#18654,#15354,#15355);
#12189=AXIS2_PLACEMENT_3D('',#18657,#15357,#15358);
#12190=AXIS2_PLACEMENT_3D('',#18658,#15359,#15360);
#12191=AXIS2_PLACEMENT_3D('',#18660,#15361,#15362);
#12192=AXIS2_PLACEMENT_3D('',#18661,#15363,#15364);
#12193=AXIS2_PLACEMENT_3D('',#18662,#15365,#15366);
#12194=AXIS2_PLACEMENT_3D('',#18664,#15367,#15368);
#12195=AXIS2_PLACEMENT_3D('',#18666,#15370,#15371);
#12196=AXIS2_PLACEMENT_3D('',#18668,#15372,#15373);
#12197=AXIS2_PLACEMENT_3D('',#18670,#15375,#15376);
#12198=AXIS2_PLACEMENT_3D('',#18672,#15377,#15378);
#12199=AXIS2_PLACEMENT_3D('',#18673,#15379,#15380);
#12200=AXIS2_PLACEMENT_3D('',#18674,#15381,#15382);
#12201=AXIS2_PLACEMENT_3D('',#18677,#15383,#15384);
#12202=AXIS2_PLACEMENT_3D('',#18678,#15385,#15386);
#12203=AXIS2_PLACEMENT_3D('',#18680,#15388,#15389);
#12204=AXIS2_PLACEMENT_3D('',#18684,#15391,#15392);
#12205=AXIS2_PLACEMENT_3D('',#18685,#15393,#15394);
#12206=AXIS2_PLACEMENT_3D('',#18686,#15395,#15396);
#12207=AXIS2_PLACEMENT_3D('',#18688,#15397,#15398);
#12208=AXIS2_PLACEMENT_3D('',#18689,#15399,#15400);
#12209=AXIS2_PLACEMENT_3D('',#18690,#15401,#15402);
#12210=AXIS2_PLACEMENT_3D('',#18692,#15403,#15404);
#12211=AXIS2_PLACEMENT_3D('',#18694,#15406,#15407);
#12212=AXIS2_PLACEMENT_3D('',#18695,#15408,#15409);
#12213=AXIS2_PLACEMENT_3D('',#18696,#15410,#15411);
#12214=AXIS2_PLACEMENT_3D('',#18698,#15412,#15413);
#12215=AXIS2_PLACEMENT_3D('',#18700,#15414,#15415);
#12216=AXIS2_PLACEMENT_3D('',#18701,#15416,#15417);
#12217=AXIS2_PLACEMENT_3D('',#18702,#15418,#15419);
#12218=AXIS2_PLACEMENT_3D('',#18704,#15420,#15421);
#12219=AXIS2_PLACEMENT_3D('',#18707,#15423,#15424);
#12220=AXIS2_PLACEMENT_3D('',#18708,#15425,#15426);
#12221=AXIS2_PLACEMENT_3D('',#18710,#15427,#15428);
#12222=AXIS2_PLACEMENT_3D('',#18712,#15430,#15431);
#12223=AXIS2_PLACEMENT_3D('',#18715,#15432,#15433);
#12224=AXIS2_PLACEMENT_3D('',#18716,#15434,#15435);
#12225=AXIS2_PLACEMENT_3D('',#18718,#15437,#15438);
#12226=AXIS2_PLACEMENT_3D('',#18721,#15440,#15441);
#12227=AXIS2_PLACEMENT_3D('',#18722,#15442,#15443);
#12228=AXIS2_PLACEMENT_3D('',#18725,#15444,#15445);
#12229=AXIS2_PLACEMENT_3D('',#18728,#15447,#15448);
#12230=AXIS2_PLACEMENT_3D('',#18729,#15449,#15450);
#12231=AXIS2_PLACEMENT_3D('',#18730,#15451,#15452);
#12232=AXIS2_PLACEMENT_3D('',#18733,#15453,#15454);
#12233=AXIS2_PLACEMENT_3D('',#18736,#15456,#15457);
#12234=AXIS2_PLACEMENT_3D('',#18737,#15458,#15459);
#12235=AXIS2_PLACEMENT_3D('',#18738,#15460,#15461);
#12236=AXIS2_PLACEMENT_3D('',#18740,#15462,#15463);
#12237=AXIS2_PLACEMENT_3D('',#18743,#15465,#15466);
#12238=AXIS2_PLACEMENT_3D('',#18744,#15467,#15468);
#12239=AXIS2_PLACEMENT_3D('',#18747,#15469,#15470);
#12240=AXIS2_PLACEMENT_3D('',#18748,#15471,#15472);
#12241=AXIS2_PLACEMENT_3D('',#18751,#15474,#15475);
#12242=AXIS2_PLACEMENT_3D('',#18752,#15476,#15477);
#12243=AXIS2_PLACEMENT_3D('',#18756,#15479,#15480);
#12244=AXIS2_PLACEMENT_3D('',#18757,#15481,#15482);
#12245=AXIS2_PLACEMENT_3D('',#18758,#15483,#15484);
#12246=AXIS2_PLACEMENT_3D('',#18760,#15486,#15487);
#12247=AXIS2_PLACEMENT_3D('',#18762,#15489,#15490);
#12248=AXIS2_PLACEMENT_3D('',#18764,#15491,#15492);
#12249=AXIS2_PLACEMENT_3D('',#18767,#15494,#15495);
#12250=AXIS2_PLACEMENT_3D('',#18768,#15496,#15497);
#12251=AXIS2_PLACEMENT_3D('',#18770,#15498,#15499);
#12252=AXIS2_PLACEMENT_3D('',#18771,#15500,#15501);
#12253=AXIS2_PLACEMENT_3D('',#18772,#15502,#15503);
#12254=AXIS2_PLACEMENT_3D('',#18774,#15504,#15505);
#12255=AXIS2_PLACEMENT_3D('',#18776,#15506,#15507);
#12256=AXIS2_PLACEMENT_3D('',#18777,#15508,#15509);
#12257=AXIS2_PLACEMENT_3D('',#18778,#15510,#15511);
#12258=AXIS2_PLACEMENT_3D('',#18780,#15512,#15513);
#12259=AXIS2_PLACEMENT_3D('',#18782,#15515,#15516);
#12260=AXIS2_PLACEMENT_3D('',#18784,#15517,#15518);
#12261=AXIS2_PLACEMENT_3D('',#18785,#15519,#15520);
#12262=AXIS2_PLACEMENT_3D('',#18786,#15521,#15522);
#12263=AXIS2_PLACEMENT_3D('',#18788,#15523,#15524);
#12264=AXIS2_PLACEMENT_3D('',#18790,#15525,#15526);
#12265=AXIS2_PLACEMENT_3D('',#18791,#15527,#15528);
#12266=AXIS2_PLACEMENT_3D('',#18792,#15529,#15530);
#12267=AXIS2_PLACEMENT_3D('',#18794,#15531,#15532);
#12268=AXIS2_PLACEMENT_3D('',#18796,#15534,#15535);
#12269=AXIS2_PLACEMENT_3D('',#18798,#15537,#15538);
#12270=AXIS2_PLACEMENT_3D('',#18799,#15539,#15540);
#12271=AXIS2_PLACEMENT_3D('',#18800,#15541,#15542);
#12272=AXIS2_PLACEMENT_3D('',#18801,#15543,#15544);
#12273=AXIS2_PLACEMENT_3D('',#18802,#15545,#15546);
#12274=AXIS2_PLACEMENT_3D('',#18803,#15547,#15548);
#12275=AXIS2_PLACEMENT_3D('',#18804,#15549,#15550);
#12276=AXIS2_PLACEMENT_3D('',#18805,#15551,#15552);
#12277=AXIS2_PLACEMENT_3D('',#18806,#15553,#15554);
#12278=AXIS2_PLACEMENT_3D('',#18807,#15555,#15556);
#12279=AXIS2_PLACEMENT_3D('',#18808,#15557,#15558);
#12280=AXIS2_PLACEMENT_3D('',#18809,#15559,#15560);
#12281=AXIS2_PLACEMENT_3D('',#18810,#15561,#15562);
#12282=AXIS2_PLACEMENT_3D('',#18811,#15563,#15564);
#12283=AXIS2_PLACEMENT_3D('',#18812,#15565,#15566);
#12284=AXIS2_PLACEMENT_3D('',#18813,#15567,#15568);
#12285=AXIS2_PLACEMENT_3D('',#18814,#15569,#15570);
#12286=AXIS2_PLACEMENT_3D('',#18815,#15571,#15572);
#12287=AXIS2_PLACEMENT_3D('',#18816,#15573,#15574);
#12288=AXIS2_PLACEMENT_3D('',#18817,#15575,#15576);
#12289=AXIS2_PLACEMENT_3D('',#18818,#15577,#15578);
#12290=AXIS2_PLACEMENT_3D('',#18819,#15579,#15580);
#12291=AXIS2_PLACEMENT_3D('',#18820,#15581,#15582);
#12292=AXIS2_PLACEMENT_3D('',#18821,#15583,#15584);
#12293=AXIS2_PLACEMENT_3D('',#18822,#15585,#15586);
#12294=AXIS2_PLACEMENT_3D('',#18823,#15587,#15588);
#12295=AXIS2_PLACEMENT_3D('',#18824,#15589,#15590);
#12296=AXIS2_PLACEMENT_3D('',#18825,#15591,#15592);
#12297=AXIS2_PLACEMENT_3D('',#18826,#15593,#15594);
#12298=AXIS2_PLACEMENT_3D('',#18827,#15595,#15596);
#12299=AXIS2_PLACEMENT_3D('',#18828,#15597,#15598);
#12300=AXIS2_PLACEMENT_3D('',#18829,#15599,#15600);
#12301=AXIS2_PLACEMENT_3D('',#18830,#15601,#15602);
#12302=AXIS2_PLACEMENT_3D('',#18831,#15603,#15604);
#12303=DIRECTION('axis',(0.,0.,1.));
#12304=DIRECTION('refdir',(1.,0.,0.));
#12305=DIRECTION('axis',(0.,0.,1.));
#12306=DIRECTION('refdir',(1.,0.,0.));
#12307=DIRECTION('center_axis',(0.,0.,-1.));
#12308=DIRECTION('ref_axis',(-1.,0.,0.));
#12309=DIRECTION('center_axis',(0.,0.,-1.));
#12310=DIRECTION('ref_axis',(-1.,0.,0.));
#12311=DIRECTION('',(0.,0.,-1.));
#12312=DIRECTION('center_axis',(0.,0.,-1.));
#12313=DIRECTION('ref_axis',(-1.,0.,0.));
#12314=DIRECTION('center_axis',(0.,0.,-1.));
#12315=DIRECTION('ref_axis',(-1.,0.,0.));
#12316=DIRECTION('center_axis',(0.,0.,-1.));
#12317=DIRECTION('ref_axis',(-1.,0.,0.));
#12318=DIRECTION('',(0.,0.,-1.));
#12319=DIRECTION('center_axis',(0.,0.,-1.));
#12320=DIRECTION('ref_axis',(-1.,0.,0.));
#12321=DIRECTION('center_axis',(0.,0.,1.));
#12322=DIRECTION('ref_axis',(1.,0.,0.));
#12323=DIRECTION('center_axis',(0.,0.,1.));
#12324=DIRECTION('ref_axis',(1.,0.,0.));
#12325=DIRECTION('',(0.,0.,1.));
#12326=DIRECTION('center_axis',(0.,0.,1.));
#12327=DIRECTION('ref_axis',(1.,0.,0.));
#12328=DIRECTION('center_axis',(0.,0.,1.));
#12329=DIRECTION('ref_axis',(1.,0.,0.));
#12330=DIRECTION('center_axis',(0.,-1.15648231731787E-16,-1.));
#12331=DIRECTION('ref_axis',(0.,1.,-1.15648231731787E-16));
#12332=DIRECTION('',(0.,0.,1.));
#12333=DIRECTION('center_axis',(0.,0.,1.));
#12334=DIRECTION('ref_axis',(1.,0.,0.));
#12335=DIRECTION('center_axis',(0.,0.,1.));
#12336=DIRECTION('ref_axis',(1.,0.,0.));
#12337=DIRECTION('center_axis',(0.,0.,1.));
#12338=DIRECTION('ref_axis',(1.,0.,0.));
#12339=DIRECTION('',(0.,0.,1.));
#12340=DIRECTION('center_axis',(0.,0.,1.));
#12341=DIRECTION('ref_axis',(1.,0.,0.));
#12342=DIRECTION('center_axis',(0.,0.,1.));
#12343=DIRECTION('ref_axis',(1.,0.,0.));
#12344=DIRECTION('center_axis',(0.,-1.15648231731787E-16,-1.));
#12345=DIRECTION('ref_axis',(0.,1.,-1.15648231731787E-16));
#12346=DIRECTION('',(0.,0.,1.));
#12347=DIRECTION('center_axis',(0.,0.,1.));
#12348=DIRECTION('ref_axis',(1.,0.,0.));
#12349=DIRECTION('center_axis',(0.,0.,-1.));
#12350=DIRECTION('ref_axis',(-1.,0.,0.));
#12351=DIRECTION('center_axis',(0.,0.,-1.));
#12352=DIRECTION('ref_axis',(-1.,0.,0.));
#12353=DIRECTION('',(0.,0.,-1.));
#12354=DIRECTION('center_axis',(0.,0.,-1.));
#12355=DIRECTION('ref_axis',(-1.,0.,0.));
#12356=DIRECTION('center_axis',(0.,0.,-1.));
#12357=DIRECTION('ref_axis',(-1.,0.,0.));
#12358=DIRECTION('center_axis',(0.,0.,-1.));
#12359=DIRECTION('ref_axis',(-1.,0.,0.));
#12360=DIRECTION('',(0.,0.,-1.));
#12361=DIRECTION('center_axis',(0.,0.,-1.));
#12362=DIRECTION('ref_axis',(-1.,0.,0.));
#12363=DIRECTION('center_axis',(0.,0.,-1.));
#12364=DIRECTION('ref_axis',(-1.,0.,0.));
#12365=DIRECTION('center_axis',(0.,0.,-1.));
#12366=DIRECTION('ref_axis',(-1.,0.,0.));
#12367=DIRECTION('',(0.,0.,-1.));
#12368=DIRECTION('center_axis',(0.,0.,-1.));
#12369=DIRECTION('ref_axis',(-1.,0.,0.));
#12370=DIRECTION('center_axis',(1.,0.,0.));
#12371=DIRECTION('ref_axis',(0.,0.,-1.));
#12372=DIRECTION('',(0.,1.15648231731787E-16,1.));
#12373=DIRECTION('',(0.,-1.,1.09792625061823E-16));
#12374=DIRECTION('',(0.,1.15648231731787E-16,1.));
#12375=DIRECTION('',(0.,1.,-1.15648231731787E-16));
#12376=DIRECTION('',(0.,0.,-1.));
#12377=DIRECTION('',(0.,1.,0.));
#12378=DIRECTION('',(0.,0.,1.));
#12379=DIRECTION('',(0.,1.,0.));
#12380=DIRECTION('',(0.,0.,1.));
#12381=DIRECTION('',(0.,1.,-1.15648231731787E-16));
#12382=DIRECTION('center_axis',(0.,1.15648231731787E-16,1.));
#12383=DIRECTION('ref_axis',(0.,-1.,1.15648231731787E-16));
#12384=DIRECTION('',(-1.,0.,0.));
#12385=DIRECTION('',(-1.,0.,0.));
#12386=DIRECTION('center_axis',(0.,-1.15648231731787E-16,-1.));
#12387=DIRECTION('ref_axis',(0.,-1.,1.15648231731787E-16));
#12388=DIRECTION('',(0.,1.,-1.15648231731787E-16));
#12389=DIRECTION('center_axis',(0.,1.15648231731787E-16,1.));
#12390=DIRECTION('ref_axis',(0.,-1.,1.15648231731787E-16));
#12391=DIRECTION('',(1.,0.,0.));
#12392=DIRECTION('',(0.,1.,-1.15648231731787E-16));
#12393=DIRECTION('center_axis',(0.,-1.15648231731787E-16,-1.));
#12394=DIRECTION('ref_axis',(0.,-1.,1.15648231731787E-16));
#12395=DIRECTION('',(-1.,0.,0.));
#12396=DIRECTION('center_axis',(0.,0.,1.));
#12397=DIRECTION('ref_axis',(1.,0.,0.));
#12398=DIRECTION('',(1.,0.,0.));
#12399=DIRECTION('',(0.86602540378444,0.499999999999998,0.));
#12400=DIRECTION('',(0.,1.,0.));
#12401=DIRECTION('',(1.,0.,0.));
#12402=DIRECTION('center_axis',(0.,0.,1.));
#12403=DIRECTION('ref_axis',(1.,0.,0.));
#12404=DIRECTION('',(-0.977786581118157,-0.209602962253079,0.));
#12405=DIRECTION('',(-0.977786581118157,-0.209602962253078,0.));
#12406=DIRECTION('',(0.,-1.,0.));
#12407=DIRECTION('',(0.,-1.,0.));
#12408=DIRECTION('',(0.866025403784439,-0.499999999999999,0.));
#12409=DIRECTION('',(0.866025403784438,0.500000000000001,0.));
#12410=DIRECTION('',(0.,1.,0.));
#12411=DIRECTION('',(-0.866025403784438,0.500000000000001,0.));
#12412=DIRECTION('',(-0.866025403784439,-0.499999999999999,0.));
#12413=DIRECTION('',(0.,1.,0.));
#12414=DIRECTION('',(-0.866025403784438,0.500000000000001,0.));
#12415=DIRECTION('',(-0.866025403784439,-0.499999999999999,0.));
#12416=DIRECTION('',(0.,-1.,0.));
#12417=DIRECTION('',(0.866025403784439,-0.499999999999999,0.));
#12418=DIRECTION('',(0.866025403784438,0.500000000000001,0.));
#12419=DIRECTION('center_axis',(0.209602962253079,-0.977786581118157,0.));
#12420=DIRECTION('ref_axis',(0.977786581118157,0.209602962253079,0.));
#12421=DIRECTION('',(0.,0.,-1.));
#12422=DIRECTION('',(-0.977786581118157,-0.209602962253079,0.));
#12423=DIRECTION('',(0.,0.,-1.));
#12424=DIRECTION('center_axis',(0.,0.,-1.));
#12425=DIRECTION('ref_axis',(0.99443113917409,0.105388374315774,0.));
#12426=DIRECTION('',(0.,0.,-1.));
#12427=DIRECTION('center_axis',(0.,0.,1.));
#12428=DIRECTION('ref_axis',(1.,0.,0.));
#12429=DIRECTION('center_axis',(0.,1.,0.));
#12430=DIRECTION('ref_axis',(0.,0.,1.));
#12431=DIRECTION('',(0.,0.,1.));
#12432=DIRECTION('',(1.,0.,0.));
#12433=DIRECTION('',(0.,0.,-1.));
#12434=DIRECTION('',(-1.,0.,0.));
#12435=DIRECTION('center_axis',(1.,0.,0.));
#12436=DIRECTION('ref_axis',(0.,0.,-1.));
#12437=DIRECTION('',(0.,0.,-1.));
#12438=DIRECTION('',(0.,1.15648231731787E-16,1.));
#12439=DIRECTION('',(0.,1.,-1.09792625061823E-16));
#12440=DIRECTION('',(0.,1.15648231731787E-16,1.));
#12441=DIRECTION('',(0.,0.,1.));
#12442=DIRECTION('',(0.,-1.,0.));
#12443=DIRECTION('center_axis',(-9.91270557701033E-17,1.,0.));
#12444=DIRECTION('ref_axis',(-1.,-9.91270557701033E-17,0.));
#12445=DIRECTION('',(0.,0.,-1.));
#12446=DIRECTION('',(1.,9.91270557701033E-17,0.));
#12447=DIRECTION('center_axis',(0.,0.,1.));
#12448=DIRECTION('ref_axis',(1.,0.,0.));
#12449=DIRECTION('center_axis',(0.,0.,1.));
#12450=DIRECTION('ref_axis',(1.,0.,0.));
#12451=DIRECTION('center_axis',(0.,0.,1.));
#12452=DIRECTION('ref_axis',(1.,0.,0.));
#12453=DIRECTION('center_axis',(0.,0.,-1.));
#12454=DIRECTION('ref_axis',(-1.,0.,0.));
#12455=DIRECTION('center_axis',(0.,0.,-1.));
#12456=DIRECTION('ref_axis',(-1.,0.,0.));
#12457=DIRECTION('center_axis',(-0.209602962253078,0.977786581118157,0.));
#12458=DIRECTION('ref_axis',(-0.977786581118157,-0.209602962253078,0.));
#12459=DIRECTION('',(-0.977786581118157,-0.209602962253078,0.));
#12460=DIRECTION('',(0.,0.,1.));
#12461=DIRECTION('center_axis',(-1.,0.,0.));
#12462=DIRECTION('ref_axis',(0.,0.,1.));
#12463=DIRECTION('',(0.,-1.,0.));
#12464=DIRECTION('',(0.,0.,1.));
#12465=DIRECTION('center_axis',(0.,0.,-1.));
#12466=DIRECTION('ref_axis',(-1.,0.,0.));
#12467=DIRECTION('',(0.,1.,0.));
#12468=DIRECTION('',(-0.86602540378444,-0.499999999999998,0.));
#12469=DIRECTION('',(-1.,0.,0.));
#12470=DIRECTION('center_axis',(0.,0.,-1.));
#12471=DIRECTION('ref_axis',(-1.,0.,0.));
#12472=DIRECTION('center_axis',(0.,0.,1.));
#12473=DIRECTION('ref_axis',(1.,0.,0.));
#12474=DIRECTION('center_axis',(0.,0.,-1.));
#12475=DIRECTION('ref_axis',(-1.,0.,0.));
#12476=DIRECTION('center_axis',(0.,0.,-1.));
#12477=DIRECTION('ref_axis',(-1.,0.,0.));
#12478=DIRECTION('center_axis',(-0.500000000000001,-0.866025403784438,0.));
#12479=DIRECTION('ref_axis',(0.866025403784438,-0.500000000000001,0.));
#12480=DIRECTION('',(0.,0.,-1.));
#12481=DIRECTION('',(-0.866025403784438,0.500000000000001,0.));
#12482=DIRECTION('',(0.,0.,-1.));
#12483=DIRECTION('center_axis',(0.499999999999999,-0.866025403784439,0.));
#12484=DIRECTION('ref_axis',(0.866025403784439,0.499999999999999,0.));
#12485=DIRECTION('',(-0.866025403784439,-0.499999999999999,0.));
#12486=DIRECTION('',(0.,0.,-1.));
#12487=DIRECTION('center_axis',(1.,0.,0.));
#12488=DIRECTION('ref_axis',(0.,0.,-1.));
#12489=DIRECTION('',(0.,-1.,0.));
#12490=DIRECTION('',(0.,0.,-1.));
#12491=DIRECTION('center_axis',(0.499999999999999,0.866025403784439,0.));
#12492=DIRECTION('ref_axis',(-0.866025403784439,0.499999999999999,0.));
#12493=DIRECTION('',(0.866025403784439,-0.499999999999999,0.));
#12494=DIRECTION('',(0.,0.,-1.));
#12495=DIRECTION('center_axis',(-0.500000000000001,0.866025403784438,0.));
#12496=DIRECTION('ref_axis',(-0.866025403784438,-0.500000000000001,0.));
#12497=DIRECTION('',(0.866025403784438,0.500000000000001,0.));
#12498=DIRECTION('',(0.,0.,-1.));
#12499=DIRECTION('center_axis',(-1.,0.,0.));
#12500=DIRECTION('ref_axis',(0.,0.,1.));
#12501=DIRECTION('',(0.,1.,0.));
#12502=DIRECTION('center_axis',(0.,0.,1.));
#12503=DIRECTION('ref_axis',(1.,0.,0.));
#12504=DIRECTION('center_axis',(0.499999999999999,0.866025403784439,0.));
#12505=DIRECTION('ref_axis',(-0.866025403784439,0.499999999999999,0.));
#12506=DIRECTION('',(0.,0.,-1.));
#12507=DIRECTION('',(0.866025403784439,-0.499999999999999,0.));
#12508=DIRECTION('',(0.,0.,-1.));
#12509=DIRECTION('center_axis',(-0.500000000000001,0.866025403784438,0.));
#12510=DIRECTION('ref_axis',(-0.866025403784438,-0.500000000000001,0.));
#12511=DIRECTION('',(0.866025403784438,0.500000000000001,0.));
#12512=DIRECTION('',(0.,0.,-1.));
#12513=DIRECTION('center_axis',(-1.,0.,0.));
#12514=DIRECTION('ref_axis',(0.,0.,1.));
#12515=DIRECTION('',(0.,1.,0.));
#12516=DIRECTION('',(0.,0.,-1.));
#12517=DIRECTION('center_axis',(-0.500000000000001,-0.866025403784438,0.));
#12518=DIRECTION('ref_axis',(0.866025403784438,-0.500000000000001,0.));
#12519=DIRECTION('',(-0.866025403784438,0.500000000000001,0.));
#12520=DIRECTION('',(0.,0.,-1.));
#12521=DIRECTION('center_axis',(0.499999999999999,-0.866025403784439,0.));
#12522=DIRECTION('ref_axis',(0.866025403784439,0.499999999999999,0.));
#12523=DIRECTION('',(-0.866025403784439,-0.499999999999999,0.));
#12524=DIRECTION('',(0.,0.,-1.));
#12525=DIRECTION('center_axis',(1.,0.,0.));
#12526=DIRECTION('ref_axis',(0.,0.,-1.));
#12527=DIRECTION('',(0.,-1.,0.));
#12528=DIRECTION('center_axis',(0.,0.,-1.));
#12529=DIRECTION('ref_axis',(-1.,0.,0.));
#12530=DIRECTION('center_axis',(0.,-1.,0.));
#12531=DIRECTION('ref_axis',(0.,0.,-1.));
#12532=DIRECTION('',(0.,0.,1.));
#12533=DIRECTION('center_axis',(1.,0.,0.));
#12534=DIRECTION('ref_axis',(0.,0.,-1.));
#12535=DIRECTION('',(0.,0.,-1.));
#12536=DIRECTION('center_axis',(-0.499999999999998,0.86602540378444,0.));
#12537=DIRECTION('ref_axis',(0.,0.,-1.));
#12538=DIRECTION('center_axis',(0.,-1.09792625061823E-16,-1.));
#12539=DIRECTION('ref_axis',(0.,1.,-1.09792625061823E-16));
#12540=DIRECTION('',(-1.,0.,0.));
#12541=DIRECTION('',(1.,0.,0.));
#12542=DIRECTION('center_axis',(0.,1.,-1.15648231731787E-16));
#12543=DIRECTION('ref_axis',(0.,1.15648231731787E-16,1.));
#12544=DIRECTION('center_axis',(0.,-1.,1.15648231731787E-16));
#12545=DIRECTION('ref_axis',(0.,-1.15648231731787E-16,-1.));
#12546=DIRECTION('axis',(0.,0.,1.));
#12547=DIRECTION('refdir',(1.,0.,0.));
#12548=DIRECTION('center_axis',(0.,0.,1.));
#12549=DIRECTION('ref_axis',(-1.,0.,0.));
#12550=DIRECTION('center_axis',(0.,0.,-1.));
#12551=DIRECTION('ref_axis',(-1.,0.,0.));
#12552=DIRECTION('',(0.,0.,1.));
#12553=DIRECTION('center_axis',(0.,0.,-1.));
#12554=DIRECTION('ref_axis',(-1.,0.,0.));
#12555=DIRECTION('center_axis',(0.,0.,1.));
#12556=DIRECTION('ref_axis',(-1.,0.,0.));
#12557=DIRECTION('center_axis',(0.,0.,-1.));
#12558=DIRECTION('ref_axis',(-1.,0.,0.));
#12559=DIRECTION('',(0.,0.,1.));
#12560=DIRECTION('center_axis',(0.,0.,-1.));
#12561=DIRECTION('ref_axis',(-1.,0.,0.));
#12562=DIRECTION('center_axis',(0.,0.,-1.));
#12563=DIRECTION('ref_axis',(1.,0.,0.));
#12564=DIRECTION('center_axis',(0.,0.,1.));
#12565=DIRECTION('ref_axis',(1.,0.,0.));
#12566=DIRECTION('',(0.,0.,-1.));
#12567=DIRECTION('center_axis',(0.,0.,1.));
#12568=DIRECTION('ref_axis',(1.,0.,0.));
#12569=DIRECTION('center_axis',(0.,0.,-1.));
#12570=DIRECTION('ref_axis',(1.,0.,0.));
#12571=DIRECTION('center_axis',(0.,1.15648231731787E-16,-1.));
#12572=DIRECTION('ref_axis',(0.,1.,1.15648231731787E-16));
#12573=DIRECTION('',(0.,0.,-1.));
#12574=DIRECTION('center_axis',(0.,0.,1.));
#12575=DIRECTION('ref_axis',(1.,0.,0.));
#12576=DIRECTION('center_axis',(0.,0.,-1.));
#12577=DIRECTION('ref_axis',(1.,0.,0.));
#12578=DIRECTION('center_axis',(0.,0.,1.));
#12579=DIRECTION('ref_axis',(1.,0.,0.));
#12580=DIRECTION('',(0.,0.,-1.));
#12581=DIRECTION('center_axis',(0.,0.,1.));
#12582=DIRECTION('ref_axis',(1.,0.,0.));
#12583=DIRECTION('center_axis',(0.,0.,-1.));
#12584=DIRECTION('ref_axis',(1.,0.,0.));
#12585=DIRECTION('center_axis',(0.,1.15648231731787E-16,-1.));
#12586=DIRECTION('ref_axis',(0.,1.,1.15648231731787E-16));
#12587=DIRECTION('',(0.,0.,-1.));
#12588=DIRECTION('center_axis',(0.,0.,1.));
#12589=DIRECTION('ref_axis',(1.,0.,0.));
#12590=DIRECTION('center_axis',(0.,0.,1.));
#12591=DIRECTION('ref_axis',(-1.,0.,0.));
#12592=DIRECTION('center_axis',(0.,0.,-1.));
#12593=DIRECTION('ref_axis',(-1.,0.,0.));
#12594=DIRECTION('',(0.,0.,1.));
#12595=DIRECTION('center_axis',(0.,0.,-1.));
#12596=DIRECTION('ref_axis',(-1.,0.,0.));
#12597=DIRECTION('center_axis',(0.,0.,1.));
#12598=DIRECTION('ref_axis',(-1.,0.,0.));
#12599=DIRECTION('center_axis',(0.,0.,-1.));
#12600=DIRECTION('ref_axis',(-1.,0.,0.));
#12601=DIRECTION('',(0.,0.,1.));
#12602=DIRECTION('center_axis',(0.,0.,-1.));
#12603=DIRECTION('ref_axis',(-1.,0.,0.));
#12604=DIRECTION('center_axis',(0.,0.,1.));
#12605=DIRECTION('ref_axis',(-1.,0.,0.));
#12606=DIRECTION('center_axis',(0.,0.,-1.));
#12607=DIRECTION('ref_axis',(-1.,0.,0.));
#12608=DIRECTION('',(0.,0.,1.));
#12609=DIRECTION('center_axis',(0.,0.,-1.));
#12610=DIRECTION('ref_axis',(-1.,0.,0.));
#12611=DIRECTION('center_axis',(1.,0.,0.));
#12612=DIRECTION('ref_axis',(0.,0.,1.));
#12613=DIRECTION('',(0.,1.15648231731787E-16,-1.));
#12614=DIRECTION('',(0.,1.,1.15648231731787E-16));
#12615=DIRECTION('',(0.,0.,-1.));
#12616=DIRECTION('',(0.,1.,0.));
#12617=DIRECTION('',(0.,0.,-1.));
#12618=DIRECTION('',(0.,1.,0.));
#12619=DIRECTION('',(0.,0.,1.));
#12620=DIRECTION('',(0.,1.,1.15648231731787E-16));
#12621=DIRECTION('',(0.,1.15648231731787E-16,-1.));
#12622=DIRECTION('',(0.,-1.,-1.09792625061823E-16));
#12623=DIRECTION('center_axis',(0.,1.15648231731787E-16,-1.));
#12624=DIRECTION('ref_axis',(0.,-1.,-1.15648231731787E-16));
#12625=DIRECTION('',(-1.,0.,0.));
#12626=DIRECTION('',(0.,1.,1.15648231731787E-16));
#12627=DIRECTION('center_axis',(0.,1.15648231731787E-16,-1.));
#12628=DIRECTION('ref_axis',(0.,-1.,-1.15648231731787E-16));
#12629=DIRECTION('',(-1.,0.,0.));
#12630=DIRECTION('center_axis',(0.,1.15648231731787E-16,-1.));
#12631=DIRECTION('ref_axis',(0.,-1.,-1.15648231731787E-16));
#12632=DIRECTION('',(1.,0.,0.));
#12633=DIRECTION('',(-1.,0.,0.));
#12634=DIRECTION('center_axis',(0.,1.15648231731787E-16,-1.));
#12635=DIRECTION('ref_axis',(0.,-1.,-1.15648231731787E-16));
#12636=DIRECTION('',(0.,1.,1.15648231731787E-16));
#12637=DIRECTION('center_axis',(0.,0.,-1.));
#12638=DIRECTION('ref_axis',(1.,0.,0.));
#12639=DIRECTION('',(1.,0.,0.));
#12640=DIRECTION('',(0.,-1.,0.));
#12641=DIRECTION('',(-0.977786581118157,-0.209602962253078,0.));
#12642=DIRECTION('',(-0.977786581118157,-0.209602962253079,0.));
#12643=DIRECTION('center_axis',(0.,0.,1.));
#12644=DIRECTION('ref_axis',(1.,0.,0.));
#12645=DIRECTION('',(1.,0.,0.));
#12646=DIRECTION('',(0.,1.,0.));
#12647=DIRECTION('',(0.86602540378444,0.499999999999998,0.));
#12648=DIRECTION('',(0.,-1.,0.));
#12649=DIRECTION('',(-0.866025403784439,-0.499999999999999,0.));
#12650=DIRECTION('',(-0.866025403784438,0.500000000000001,0.));
#12651=DIRECTION('',(0.,1.,0.));
#12652=DIRECTION('',(0.866025403784438,0.500000000000001,0.));
#12653=DIRECTION('',(0.866025403784439,-0.499999999999999,0.));
#12654=DIRECTION('',(0.,1.,0.));
#12655=DIRECTION('',(0.866025403784438,0.500000000000001,0.));
#12656=DIRECTION('',(0.866025403784439,-0.499999999999999,0.));
#12657=DIRECTION('',(0.,-1.,0.));
#12658=DIRECTION('',(-0.866025403784439,-0.499999999999999,0.));
#12659=DIRECTION('',(-0.866025403784438,0.500000000000001,0.));
#12660=DIRECTION('center_axis',(0.209602962253079,-0.977786581118157,0.));
#12661=DIRECTION('ref_axis',(0.977786581118157,0.209602962253079,0.));
#12662=DIRECTION('',(0.,0.,1.));
#12663=DIRECTION('',(-0.977786581118157,-0.209602962253079,0.));
#12664=DIRECTION('',(0.,0.,1.));
#12665=DIRECTION('center_axis',(0.,0.,1.));
#12666=DIRECTION('ref_axis',(0.99443113917409,0.105388374315774,0.));
#12667=DIRECTION('center_axis',(0.,0.,1.));
#12668=DIRECTION('ref_axis',(1.,0.,0.));
#12669=DIRECTION('',(0.,0.,1.));
#12670=DIRECTION('center_axis',(0.,1.,0.));
#12671=DIRECTION('ref_axis',(0.,0.,-1.));
#12672=DIRECTION('',(-1.,0.,0.));
#12673=DIRECTION('',(0.,0.,1.));
#12674=DIRECTION('',(1.,0.,0.));
#12675=DIRECTION('',(0.,0.,-1.));
#12676=DIRECTION('center_axis',(1.,0.,0.));
#12677=DIRECTION('ref_axis',(0.,0.,1.));
#12678=DIRECTION('',(0.,0.,1.));
#12679=DIRECTION('',(0.,-1.,0.));
#12680=DIRECTION('',(0.,0.,-1.));
#12681=DIRECTION('',(0.,1.15648231731787E-16,-1.));
#12682=DIRECTION('',(0.,1.,1.09792625061823E-16));
#12683=DIRECTION('',(0.,1.15648231731787E-16,-1.));
#12684=DIRECTION('center_axis',(-9.91270557701033E-17,1.,0.));
#12685=DIRECTION('ref_axis',(-1.,-9.91270557701033E-17,0.));
#12686=DIRECTION('',(0.,0.,1.));
#12687=DIRECTION('',(1.,9.91270557701033E-17,0.));
#12688=DIRECTION('center_axis',(0.,0.,-1.));
#12689=DIRECTION('ref_axis',(1.,0.,0.));
#12690=DIRECTION('center_axis',(0.,0.,1.));
#12691=DIRECTION('ref_axis',(1.,0.,0.));
#12692=DIRECTION('center_axis',(0.,0.,1.));
#12693=DIRECTION('ref_axis',(1.,0.,0.));
#12694=DIRECTION('center_axis',(0.,0.,1.));
#12695=DIRECTION('ref_axis',(-1.,0.,0.));
#12696=DIRECTION('center_axis',(0.,0.,1.));
#12697=DIRECTION('ref_axis',(-1.,0.,0.));
#12698=DIRECTION('center_axis',(-0.209602962253078,0.977786581118157,0.));
#12699=DIRECTION('ref_axis',(-0.977786581118157,-0.209602962253078,0.));
#12700=DIRECTION('',(0.,0.,-1.));
#12701=DIRECTION('',(-0.977786581118157,-0.209602962253078,0.));
#12702=DIRECTION('center_axis',(-1.,0.,0.));
#12703=DIRECTION('ref_axis',(0.,0.,-1.));
#12704=DIRECTION('',(0.,-1.,0.));
#12705=DIRECTION('',(0.,0.,-1.));
#12706=DIRECTION('center_axis',(0.,0.,1.));
#12707=DIRECTION('ref_axis',(-1.,0.,0.));
#12708=DIRECTION('',(0.,1.,0.));
#12709=DIRECTION('',(-1.,0.,0.));
#12710=DIRECTION('',(-0.86602540378444,-0.499999999999998,0.));
#12711=DIRECTION('center_axis',(0.,0.,1.));
#12712=DIRECTION('ref_axis',(-1.,0.,0.));
#12713=DIRECTION('center_axis',(0.,0.,-1.));
#12714=DIRECTION('ref_axis',(1.,0.,0.));
#12715=DIRECTION('center_axis',(0.,0.,1.));
#12716=DIRECTION('ref_axis',(-1.,0.,0.));
#12717=DIRECTION('center_axis',(0.,0.,1.));
#12718=DIRECTION('ref_axis',(-1.,0.,0.));
#12719=DIRECTION('center_axis',(-0.500000000000001,-0.866025403784438,0.));
#12720=DIRECTION('ref_axis',(0.866025403784438,-0.500000000000001,0.));
#12721=DIRECTION('',(0.,0.,1.));
#12722=DIRECTION('',(-0.866025403784438,0.500000000000001,0.));
#12723=DIRECTION('',(0.,0.,1.));
#12724=DIRECTION('center_axis',(0.499999999999999,-0.866025403784439,0.));
#12725=DIRECTION('ref_axis',(0.866025403784439,0.499999999999999,0.));
#12726=DIRECTION('',(0.,0.,1.));
#12727=DIRECTION('',(-0.866025403784439,-0.499999999999999,0.));
#12728=DIRECTION('center_axis',(1.,0.,0.));
#12729=DIRECTION('ref_axis',(0.,0.,1.));
#12730=DIRECTION('',(0.,0.,1.));
#12731=DIRECTION('',(0.,-1.,0.));
#12732=DIRECTION('center_axis',(0.499999999999999,0.866025403784439,0.));
#12733=DIRECTION('ref_axis',(-0.866025403784439,0.499999999999999,0.));
#12734=DIRECTION('',(0.,0.,1.));
#12735=DIRECTION('',(0.866025403784439,-0.499999999999999,0.));
#12736=DIRECTION('center_axis',(-0.500000000000001,0.866025403784438,0.));
#12737=DIRECTION('ref_axis',(-0.866025403784438,-0.500000000000001,0.));
#12738=DIRECTION('',(0.,0.,1.));
#12739=DIRECTION('',(0.866025403784438,0.500000000000001,0.));
#12740=DIRECTION('center_axis',(-1.,0.,0.));
#12741=DIRECTION('ref_axis',(0.,0.,-1.));
#12742=DIRECTION('',(0.,1.,0.));
#12743=DIRECTION('center_axis',(0.,0.,-1.));
#12744=DIRECTION('ref_axis',(1.,0.,0.));
#12745=DIRECTION('center_axis',(0.499999999999999,0.866025403784439,0.));
#12746=DIRECTION('ref_axis',(-0.866025403784439,0.499999999999999,0.));
#12747=DIRECTION('',(0.,0.,1.));
#12748=DIRECTION('',(0.866025403784439,-0.499999999999999,0.));
#12749=DIRECTION('',(0.,0.,1.));
#12750=DIRECTION('center_axis',(-0.500000000000001,0.866025403784438,0.));
#12751=DIRECTION('ref_axis',(-0.866025403784438,-0.500000000000001,0.));
#12752=DIRECTION('',(0.,0.,1.));
#12753=DIRECTION('',(0.866025403784438,0.500000000000001,0.));
#12754=DIRECTION('center_axis',(-1.,0.,0.));
#12755=DIRECTION('ref_axis',(0.,0.,-1.));
#12756=DIRECTION('',(0.,0.,1.));
#12757=DIRECTION('',(0.,1.,0.));
#12758=DIRECTION('center_axis',(-0.500000000000001,-0.866025403784438,0.));
#12759=DIRECTION('ref_axis',(0.866025403784438,-0.500000000000001,0.));
#12760=DIRECTION('',(0.,0.,1.));
#12761=DIRECTION('',(-0.866025403784438,0.500000000000001,0.));
#12762=DIRECTION('center_axis',(0.499999999999999,-0.866025403784439,0.));
#12763=DIRECTION('ref_axis',(0.866025403784439,0.499999999999999,0.));
#12764=DIRECTION('',(0.,0.,1.));
#12765=DIRECTION('',(-0.866025403784439,-0.499999999999999,0.));
#12766=DIRECTION('center_axis',(1.,0.,0.));
#12767=DIRECTION('ref_axis',(0.,0.,1.));
#12768=DIRECTION('',(0.,-1.,0.));
#12769=DIRECTION('center_axis',(0.,0.,1.));
#12770=DIRECTION('ref_axis',(-1.,0.,0.));
#12771=DIRECTION('center_axis',(0.,-1.,0.));
#12772=DIRECTION('ref_axis',(0.,0.,1.));
#12773=DIRECTION('',(0.,0.,-1.));
#12774=DIRECTION('center_axis',(1.,0.,0.));
#12775=DIRECTION('ref_axis',(0.,0.,1.));
#12776=DIRECTION('',(0.,0.,1.));
#12777=DIRECTION('center_axis',(-0.499999999999998,0.86602540378444,0.));
#12778=DIRECTION('ref_axis',(0.,0.,1.));
#12779=DIRECTION('center_axis',(0.,-1.09792625061823E-16,1.));
#12780=DIRECTION('ref_axis',(0.,1.,1.09792625061823E-16));
#12781=DIRECTION('',(1.,0.,0.));
#12782=DIRECTION('',(-1.,0.,0.));
#12783=DIRECTION('center_axis',(0.,1.,1.15648231731787E-16));
#12784=DIRECTION('ref_axis',(0.,1.15648231731787E-16,-1.));
#12785=DIRECTION('center_axis',(0.,-1.,-1.15648231731787E-16));
#12786=DIRECTION('ref_axis',(0.,-1.15648231731787E-16,1.));
#12787=DIRECTION('axis',(0.,0.,1.));
#12788=DIRECTION('refdir',(1.,0.,0.));
#12789=DIRECTION('center_axis',(0.,0.,-1.));
#12790=DIRECTION('ref_axis',(1.,0.,0.));
#12791=DIRECTION('center_axis',(0.,0.,1.));
#12792=DIRECTION('ref_axis',(1.,0.,0.));
#12793=DIRECTION('',(0.,0.,-1.));
#12794=DIRECTION('center_axis',(-0.866025403784435,4.41270772476077E-16,
0.500000000000006));
#12795=DIRECTION('ref_axis',(0.500000000000006,5.55042661661472E-14,0.866025403784435));
#12796=DIRECTION('center_axis',(0.,0.,1.));
#12797=DIRECTION('ref_axis',(1.,0.,0.));
#12798=DIRECTION('center_axis',(-0.866025403784435,4.41270772476077E-16,
0.500000000000006));
#12799=DIRECTION('ref_axis',(0.500000000000006,5.55042661661472E-14,0.866025403784435));
#12800=DIRECTION('center_axis',(0.,0.,-1.));
#12801=DIRECTION('ref_axis',(1.,0.,0.));
#12802=DIRECTION('center_axis',(0.,0.,-1.));
#12803=DIRECTION('ref_axis',(-1.,0.,0.));
#12804=DIRECTION('',(0.,0.,-1.));
#12805=DIRECTION('center_axis',(0.,0.,1.));
#12806=DIRECTION('ref_axis',(1.,0.,0.));
#12807=DIRECTION('center_axis',(0.,0.,-1.));
#12808=DIRECTION('ref_axis',(1.,0.,0.));
#12809=DIRECTION('center_axis',(0.,0.,1.));
#12810=DIRECTION('ref_axis',(1.,0.,0.));
#12811=DIRECTION('',(0.,0.,-1.));
#12812=DIRECTION('center_axis',(0.,0.,1.));
#12813=DIRECTION('ref_axis',(1.,0.,0.));
#12814=DIRECTION('center_axis',(0.,0.,-1.));
#12815=DIRECTION('ref_axis',(1.,0.,0.));
#12816=DIRECTION('center_axis',(0.,0.,-1.));
#12817=DIRECTION('ref_axis',(-1.,0.,0.));
#12818=DIRECTION('',(0.,0.,-1.));
#12819=DIRECTION('center_axis',(0.,0.,1.));
#12820=DIRECTION('ref_axis',(1.,0.,0.));
#12821=DIRECTION('center_axis',(0.,0.,1.));
#12822=DIRECTION('ref_axis',(-1.,0.,0.));
#12823=DIRECTION('center_axis',(0.,0.,-1.));
#12824=DIRECTION('ref_axis',(-1.,0.,0.));
#12825=DIRECTION('',(0.,0.,1.));
#12826=DIRECTION('center_axis',(0.,0.,-1.));
#12827=DIRECTION('ref_axis',(-1.,0.,0.));
#12828=DIRECTION('center_axis',(0.,0.,1.));
#12829=DIRECTION('ref_axis',(-1.,0.,0.));
#12830=DIRECTION('center_axis',(0.,0.,-1.));
#12831=DIRECTION('ref_axis',(-1.,0.,0.));
#12832=DIRECTION('',(0.,0.,1.));
#12833=DIRECTION('center_axis',(0.,0.,-1.));
#12834=DIRECTION('ref_axis',(-1.,0.,0.));
#12835=DIRECTION('center_axis',(0.,0.,1.));
#12836=DIRECTION('ref_axis',(-1.,0.,0.));
#12837=DIRECTION('center_axis',(0.,0.,-1.));
#12838=DIRECTION('ref_axis',(-1.,0.,0.));
#12839=DIRECTION('',(0.,0.,1.));
#12840=DIRECTION('center_axis',(0.,0.,-1.));
#12841=DIRECTION('ref_axis',(-1.,0.,0.));
#12842=DIRECTION('center_axis',(0.,0.,-1.));
#12843=DIRECTION('ref_axis',(1.,0.,0.));
#12844=DIRECTION('',(1.,0.,0.));
#12845=DIRECTION('',(0.,1.,0.));
#12846=DIRECTION('',(1.,0.,0.));
#12847=DIRECTION('center_axis',(0.,0.,-1.));
#12848=DIRECTION('ref_axis',(1.,0.,0.));
#12849=DIRECTION('',(0.,1.,0.));
#12850=DIRECTION('center_axis',(0.,0.,-1.));
#12851=DIRECTION('ref_axis',(1.,0.,0.));
#12852=DIRECTION('',(-1.,-2.89120579329468E-17,0.));
#12853=DIRECTION('',(0.,1.,0.));
#12854=DIRECTION('center_axis',(0.,0.,-1.));
#12855=DIRECTION('ref_axis',(1.,0.,0.));
#12856=DIRECTION('',(1.,0.,0.));
#12857=DIRECTION('',(0.,1.,0.));
#12858=DIRECTION('center_axis',(1.,0.,0.));
#12859=DIRECTION('ref_axis',(0.,0.,1.));
#12860=DIRECTION('',(0.,0.,-1.));
#12861=DIRECTION('',(0.,-1.,0.));
#12862=DIRECTION('',(0.,0.,-1.));
#12863=DIRECTION('',(0.,0.,1.));
#12864=DIRECTION('',(0.,1.,0.));
#12865=DIRECTION('',(0.,0.,1.));
#12866=DIRECTION('center_axis',(0.227131156084319,-0.973864178382079,0.));
#12867=DIRECTION('ref_axis',(0.973864178382079,0.227131156084319,0.));
#12868=DIRECTION('',(-0.973864178382078,-0.227131156084319,0.));
#12869=DIRECTION('',(0.,0.,1.));
#12870=DIRECTION('',(-0.973864178382078,-0.227131156084319,0.));
#12871=DIRECTION('',(0.,0.,1.));
#12872=DIRECTION('center_axis',(0.,0.,1.));
#12873=DIRECTION('ref_axis',(0.993444557683537,0.114314963189256,0.));
#12874=DIRECTION('center_axis',(0.,0.,1.));
#12875=DIRECTION('ref_axis',(1.,0.,0.));
#12876=DIRECTION('center_axis',(0.,0.,1.));
#12877=DIRECTION('ref_axis',(1.,0.,0.));
#12878=DIRECTION('',(0.,0.,1.));
#12879=DIRECTION('center_axis',(0.,1.,0.));
#12880=DIRECTION('ref_axis',(0.,0.,-1.));
#12881=DIRECTION('',(1.,0.,0.));
#12882=DIRECTION('',(1.,0.,0.));
#12883=DIRECTION('',(0.,0.,-1.));
#12884=DIRECTION('center_axis',(1.,0.,0.));
#12885=DIRECTION('ref_axis',(0.,0.,1.));
#12886=DIRECTION('',(0.,0.,1.));
#12887=DIRECTION('',(0.,-1.,0.));
#12888=DIRECTION('',(0.,0.,1.));
#12889=DIRECTION('center_axis',(1.,0.,0.));
#12890=DIRECTION('ref_axis',(0.,0.,1.));
#12891=DIRECTION('',(0.,-1.,0.));
#12892=DIRECTION('center_axis',(1.,0.,0.));
#12893=DIRECTION('ref_axis',(0.,0.,1.));
#12894=DIRECTION('',(0.,0.,1.));
#12895=DIRECTION('',(0.,-1.,0.));
#12896=DIRECTION('',(0.,0.,-1.));
#12897=DIRECTION('',(0.,0.,-1.));
#12898=DIRECTION('',(0.,1.,0.));
#12899=DIRECTION('',(0.,0.,-1.));
#12900=DIRECTION('center_axis',(-1.15648231731787E-16,1.,0.));
#12901=DIRECTION('ref_axis',(-1.,-1.15648231731787E-16,0.));
#12902=DIRECTION('',(0.,0.,1.));
#12903=DIRECTION('',(1.,1.15648231731787E-16,0.));
#12904=DIRECTION('center_axis',(0.,0.,-1.));
#12905=DIRECTION('ref_axis',(1.,0.,0.));
#12906=DIRECTION('',(-1.,-1.23908819712629E-16,0.));
#12907=DIRECTION('center_axis',(0.,0.,1.));
#12908=DIRECTION('ref_axis',(1.,0.,0.));
#12909=DIRECTION('center_axis',(0.,0.,1.));
#12910=DIRECTION('ref_axis',(1.,0.,0.));
#12911=DIRECTION('',(1.,1.23908819712629E-16,0.));
#12912=DIRECTION('',(0.,-1.,0.));
#12913=DIRECTION('',(0.,-1.,0.));
#12914=DIRECTION('center_axis',(0.,0.,-1.));
#12915=DIRECTION('ref_axis',(1.,0.,0.));
#12916=DIRECTION('center_axis',(0.,0.,1.));
#12917=DIRECTION('ref_axis',(-1.,0.,0.));
#12918=DIRECTION('center_axis',(0.,0.,1.));
#12919=DIRECTION('ref_axis',(-1.,0.,0.));
#12920=DIRECTION('center_axis',(0.,0.,1.));
#12921=DIRECTION('ref_axis',(-1.,0.,0.));
#12922=DIRECTION('center_axis',(0.,0.,-1.));
#12923=DIRECTION('ref_axis',(1.,0.,0.));
#12924=DIRECTION('center_axis',(0.,0.,1.));
#12925=DIRECTION('ref_axis',(-1.,0.,0.));
#12926=DIRECTION('center_axis',(0.,0.,1.));
#12927=DIRECTION('ref_axis',(-1.,0.,0.));
#12928=DIRECTION('center_axis',(-1.23908819712629E-16,1.,0.));
#12929=DIRECTION('ref_axis',(-1.,-1.23908819712629E-16,0.));
#12930=DIRECTION('',(0.,0.,1.));
#12931=DIRECTION('',(-0.500000000000005,-6.19544098563151E-17,-0.866025403784436));
#12932=DIRECTION('',(-1.,-1.23908819712629E-16,0.));
#12933=DIRECTION('center_axis',(-1.,0.,0.));
#12934=DIRECTION('ref_axis',(0.,0.,-1.));
#12935=DIRECTION('center_axis',(-1.,0.,0.));
#12936=DIRECTION('ref_axis',(0.,0.,-1.));
#12937=DIRECTION('',(0.,1.,0.));
#12938=DIRECTION('center_axis',(-1.,0.,0.));
#12939=DIRECTION('ref_axis',(0.,0.,-1.));
#12940=DIRECTION('',(0.,0.,1.));
#12941=DIRECTION('',(0.,1.,0.));
#12942=DIRECTION('center_axis',(1.23908819712629E-16,-1.,0.));
#12943=DIRECTION('ref_axis',(1.,1.23908819712629E-16,0.));
#12944=DIRECTION('',(0.500000000000005,6.19544098563151E-17,0.866025403784436));
#12945=DIRECTION('',(1.,1.23908819712629E-16,0.));
#12946=DIRECTION('center_axis',(0.,0.,-1.));
#12947=DIRECTION('ref_axis',(1.,0.,0.));
#12948=DIRECTION('',(1.,1.23908819712629E-16,0.));
#12949=DIRECTION('',(-1.,-1.23908819712629E-16,0.));
#12950=DIRECTION('center_axis',(1.,1.23908819712629E-16,0.));
#12951=DIRECTION('ref_axis',(-1.23908819712629E-16,1.,0.));
#12952=DIRECTION('center_axis',(-1.,-1.23908819712629E-16,0.));
#12953=DIRECTION('ref_axis',(1.23908819712629E-16,-1.,0.));
#12954=DIRECTION('center_axis',(-0.866025403784436,0.,0.500000000000005));
#12955=DIRECTION('ref_axis',(0.,1.,0.));
#12956=DIRECTION('center_axis',(0.,0.,-1.));
#12957=DIRECTION('ref_axis',(1.,0.,0.));
#12958=DIRECTION('',(-1.,-2.89120579329468E-17,0.));
#12959=DIRECTION('',(1.,0.,0.));
#12960=DIRECTION('center_axis',(0.,-1.,0.));
#12961=DIRECTION('ref_axis',(0.,0.,1.));
#12962=DIRECTION('center_axis',(-2.89120579329468E-17,1.,0.));
#12963=DIRECTION('ref_axis',(-1.,-2.89120579329468E-17,0.));
#12964=DIRECTION('axis',(0.,0.,1.));
#12965=DIRECTION('refdir',(1.,0.,0.));
#12966=DIRECTION('center_axis',(0.,0.,1.));
#12967=DIRECTION('ref_axis',(1.,0.,0.));
#12968=DIRECTION('center_axis',(0.,0.,1.));
#12969=DIRECTION('ref_axis',(1.,0.,0.));
#12970=DIRECTION('',(0.,0.,1.));
#12971=DIRECTION('center_axis',(0.866025403784445,2.62556109623269E-14,
0.499999999999989));
#12972=DIRECTION('ref_axis',(0.499999999999989,-1.95567765134161E-14,-0.866025403784445));
#12973=DIRECTION('center_axis',(0.,0.,1.));
#12974=DIRECTION('ref_axis',(1.,0.,0.));
#12975=DIRECTION('center_axis',(0.866025403784445,2.62556109623269E-14,
0.499999999999989));
#12976=DIRECTION('ref_axis',(0.499999999999989,-1.95567765134161E-14,-0.866025403784445));
#12977=DIRECTION('center_axis',(0.,0.,1.));
#12978=DIRECTION('ref_axis',(1.,0.,0.));
#12979=DIRECTION('center_axis',(0.,0.,-1.));
#12980=DIRECTION('ref_axis',(-1.,0.,0.));
#12981=DIRECTION('',(0.,0.,1.));
#12982=DIRECTION('center_axis',(0.,0.,1.));
#12983=DIRECTION('ref_axis',(1.,0.,0.));
#12984=DIRECTION('center_axis',(0.,0.,1.));
#12985=DIRECTION('ref_axis',(1.,0.,0.));
#12986=DIRECTION('center_axis',(0.,0.,1.));
#12987=DIRECTION('ref_axis',(1.,0.,0.));
#12988=DIRECTION('',(0.,0.,1.));
#12989=DIRECTION('center_axis',(0.,0.,1.));
#12990=DIRECTION('ref_axis',(1.,0.,0.));
#12991=DIRECTION('center_axis',(0.,0.,1.));
#12992=DIRECTION('ref_axis',(1.,0.,0.));
#12993=DIRECTION('center_axis',(0.,0.,-1.));
#12994=DIRECTION('ref_axis',(-1.,0.,0.));
#12995=DIRECTION('',(0.,0.,1.));
#12996=DIRECTION('center_axis',(0.,0.,1.));
#12997=DIRECTION('ref_axis',(1.,0.,0.));
#12998=DIRECTION('center_axis',(0.,0.,-1.));
#12999=DIRECTION('ref_axis',(-1.,0.,0.));
#13000=DIRECTION('center_axis',(0.,0.,-1.));
#13001=DIRECTION('ref_axis',(-1.,0.,0.));
#13002=DIRECTION('',(0.,0.,-1.));
#13003=DIRECTION('center_axis',(0.,0.,-1.));
#13004=DIRECTION('ref_axis',(-1.,0.,0.));
#13005=DIRECTION('center_axis',(0.,0.,-1.));
#13006=DIRECTION('ref_axis',(-1.,0.,0.));
#13007=DIRECTION('center_axis',(0.,0.,-1.));
#13008=DIRECTION('ref_axis',(-1.,0.,0.));
#13009=DIRECTION('',(0.,0.,-1.));
#13010=DIRECTION('center_axis',(0.,0.,-1.));
#13011=DIRECTION('ref_axis',(-1.,0.,0.));
#13012=DIRECTION('center_axis',(0.,0.,-1.));
#13013=DIRECTION('ref_axis',(-1.,0.,0.));
#13014=DIRECTION('center_axis',(0.,0.,-1.));
#13015=DIRECTION('ref_axis',(-1.,0.,0.));
#13016=DIRECTION('',(0.,0.,-1.));
#13017=DIRECTION('center_axis',(0.,0.,-1.));
#13018=DIRECTION('ref_axis',(-1.,0.,0.));
#13019=DIRECTION('center_axis',(0.,0.,1.));
#13020=DIRECTION('ref_axis',(1.,0.,0.));
#13021=DIRECTION('',(1.,0.,0.));
#13022=DIRECTION('',(0.,1.,0.));
#13023=DIRECTION('center_axis',(0.,0.,-1.));
#13024=DIRECTION('ref_axis',(1.,0.,0.));
#13025=DIRECTION('',(1.,0.,0.));
#13026=DIRECTION('',(0.,1.,0.));
#13027=DIRECTION('center_axis',(0.,0.,1.));
#13028=DIRECTION('ref_axis',(1.,0.,0.));
#13029=DIRECTION('',(-1.,-2.89120579329468E-17,0.));
#13030=DIRECTION('',(0.,1.,0.));
#13031=DIRECTION('',(1.,0.,0.));
#13032=DIRECTION('center_axis',(0.,0.,-1.));
#13033=DIRECTION('ref_axis',(1.,0.,0.));
#13034=DIRECTION('',(0.,1.,0.));
#13035=DIRECTION('center_axis',(1.,0.,0.));
#13036=DIRECTION('ref_axis',(0.,0.,-1.));
#13037=DIRECTION('',(0.,0.,1.));
#13038=DIRECTION('',(0.,0.,-1.));
#13039=DIRECTION('',(0.,1.,0.));
#13040=DIRECTION('',(0.,0.,-1.));
#13041=DIRECTION('',(0.,0.,1.));
#13042=DIRECTION('',(0.,-1.,0.));
#13043=DIRECTION('center_axis',(0.227131156084319,-0.973864178382079,0.));
#13044=DIRECTION('ref_axis',(0.973864178382079,0.227131156084319,0.));
#13045=DIRECTION('',(-0.973864178382078,-0.227131156084319,0.));
#13046=DIRECTION('',(0.,0.,-1.));
#13047=DIRECTION('',(-0.973864178382078,-0.227131156084319,0.));
#13048=DIRECTION('',(0.,0.,-1.));
#13049=DIRECTION('center_axis',(0.,0.,-1.));
#13050=DIRECTION('ref_axis',(0.993444557683537,0.114314963189256,0.));
#13051=DIRECTION('center_axis',(0.,0.,1.));
#13052=DIRECTION('ref_axis',(1.,0.,0.));
#13053=DIRECTION('',(0.,0.,-1.));
#13054=DIRECTION('center_axis',(0.,0.,1.));
#13055=DIRECTION('ref_axis',(1.,0.,0.));
#13056=DIRECTION('center_axis',(0.,1.,0.));
#13057=DIRECTION('ref_axis',(0.,0.,1.));
#13058=DIRECTION('',(0.,0.,1.));
#13059=DIRECTION('',(1.,0.,0.));
#13060=DIRECTION('',(1.,0.,0.));
#13061=DIRECTION('center_axis',(1.,0.,0.));
#13062=DIRECTION('ref_axis',(0.,0.,-1.));
#13063=DIRECTION('',(0.,0.,-1.));
#13064=DIRECTION('',(0.,0.,1.));
#13065=DIRECTION('',(0.,1.,0.));
#13066=DIRECTION('',(0.,0.,1.));
#13067=DIRECTION('',(0.,0.,1.));
#13068=DIRECTION('',(0.,-1.,0.));
#13069=DIRECTION('',(0.,0.,-1.));
#13070=DIRECTION('center_axis',(-1.,0.,0.));
#13071=DIRECTION('ref_axis',(0.,0.,-1.));
#13072=DIRECTION('',(0.,-1.,0.));
#13073=DIRECTION('center_axis',(-1.,0.,0.));
#13074=DIRECTION('ref_axis',(0.,0.,-1.));
#13075=DIRECTION('',(0.,0.,-1.));
#13076=DIRECTION('',(0.,-1.,0.));
#13077=DIRECTION('center_axis',(-1.15648231731787E-16,1.,0.));
#13078=DIRECTION('ref_axis',(-1.,-1.15648231731787E-16,0.));
#13079=DIRECTION('',(0.,0.,-1.));
#13080=DIRECTION('',(1.,1.15648231731787E-16,0.));
#13081=DIRECTION('center_axis',(0.,0.,1.));
#13082=DIRECTION('ref_axis',(1.,0.,0.));
#13083=DIRECTION('',(-1.,-1.23908819712629E-16,0.));
#13084=DIRECTION('',(0.,-1.,0.));
#13085=DIRECTION('',(0.,-1.,0.));
#13086=DIRECTION('',(1.,1.23908819712629E-16,0.));
#13087=DIRECTION('center_axis',(0.,0.,1.));
#13088=DIRECTION('ref_axis',(1.,0.,0.));
#13089=DIRECTION('center_axis',(0.,0.,1.));
#13090=DIRECTION('ref_axis',(1.,0.,0.));
#13091=DIRECTION('center_axis',(0.,0.,1.));
#13092=DIRECTION('ref_axis',(1.,0.,0.));
#13093=DIRECTION('center_axis',(0.,0.,-1.));
#13094=DIRECTION('ref_axis',(-1.,0.,0.));
#13095=DIRECTION('center_axis',(0.,0.,-1.));
#13096=DIRECTION('ref_axis',(-1.,0.,0.));
#13097=DIRECTION('center_axis',(0.,0.,-1.));
#13098=DIRECTION('ref_axis',(-1.,0.,0.));
#13099=DIRECTION('center_axis',(0.,0.,1.));
#13100=DIRECTION('ref_axis',(1.,0.,0.));
#13101=DIRECTION('center_axis',(0.,0.,-1.));
#13102=DIRECTION('ref_axis',(-1.,0.,0.));
#13103=DIRECTION('center_axis',(0.,0.,-1.));
#13104=DIRECTION('ref_axis',(-1.,0.,0.));
#13105=DIRECTION('center_axis',(-1.23908819712629E-16,1.,0.));
#13106=DIRECTION('ref_axis',(-1.,-1.23908819712629E-16,0.));
#13107=DIRECTION('',(0.,0.,-1.));
#13108=DIRECTION('',(-1.,-1.23908819712629E-16,0.));
#13109=DIRECTION('',(-0.500000000000005,-6.19544098563151E-17,0.866025403784436));
#13110=DIRECTION('center_axis',(-1.,0.,0.));
#13111=DIRECTION('ref_axis',(0.,0.,1.));
#13112=DIRECTION('',(0.,1.,0.));
#13113=DIRECTION('',(0.,0.,-1.));
#13114=DIRECTION('center_axis',(1.,0.,0.));
#13115=DIRECTION('ref_axis',(0.,0.,1.));
#13116=DIRECTION('',(0.,1.,0.));
#13117=DIRECTION('center_axis',(1.,0.,0.));
#13118=DIRECTION('ref_axis',(0.,0.,1.));
#13119=DIRECTION('center_axis',(1.23908819712629E-16,-1.,0.));
#13120=DIRECTION('ref_axis',(1.,1.23908819712629E-16,0.));
#13121=DIRECTION('',(1.,1.23908819712629E-16,0.));
#13122=DIRECTION('',(0.500000000000005,6.19544098563151E-17,-0.866025403784436));
#13123=DIRECTION('center_axis',(0.,0.,1.));
#13124=DIRECTION('ref_axis',(1.,0.,0.));
#13125=DIRECTION('',(-1.,-1.23908819712629E-16,0.));
#13126=DIRECTION('',(1.,1.23908819712629E-16,0.));
#13127=DIRECTION('center_axis',(1.,1.23908819712629E-16,0.));
#13128=DIRECTION('ref_axis',(-1.23908819712629E-16,1.,0.));
#13129=DIRECTION('center_axis',(-1.,-1.23908819712629E-16,0.));
#13130=DIRECTION('ref_axis',(1.23908819712629E-16,-1.,0.));
#13131=DIRECTION('center_axis',(-0.866025403784436,0.,-0.500000000000005));
#13132=DIRECTION('ref_axis',(0.,1.,0.));
#13133=DIRECTION('center_axis',(0.,0.,1.));
#13134=DIRECTION('ref_axis',(1.,0.,0.));
#13135=DIRECTION('',(1.,0.,0.));
#13136=DIRECTION('',(-1.,-2.89120579329468E-17,0.));
#13137=DIRECTION('center_axis',(0.,-1.,0.));
#13138=DIRECTION('ref_axis',(0.,0.,-1.));
#13139=DIRECTION('center_axis',(-2.89120579329468E-17,1.,0.));
#13140=DIRECTION('ref_axis',(-1.,-2.89120579329468E-17,0.));
#13141=DIRECTION('axis',(0.,0.,1.));
#13142=DIRECTION('refdir',(1.,0.,0.));
#13143=DIRECTION('center_axis',(0.,0.,1.));
#13144=DIRECTION('ref_axis',(1.,0.,0.));
#13145=DIRECTION('center_axis',(0.,0.,1.));
#13146=DIRECTION('ref_axis',(1.,0.,0.));
#13147=DIRECTION('',(0.,0.,1.));
#13148=DIRECTION('center_axis',(0.,0.,1.));
#13149=DIRECTION('ref_axis',(1.,0.,0.));
#13150=DIRECTION('center_axis',(0.,0.,1.));
#13151=DIRECTION('ref_axis',(1.,0.,0.));
#13152=DIRECTION('center_axis',(0.,0.,1.));
#13153=DIRECTION('ref_axis',(1.,0.,0.));
#13154=DIRECTION('',(0.,0.,1.));
#13155=DIRECTION('center_axis',(0.,0.,1.));
#13156=DIRECTION('ref_axis',(1.,0.,0.));
#13157=DIRECTION('center_axis',(0.,0.,1.));
#13158=DIRECTION('ref_axis',(1.,0.,0.));
#13159=DIRECTION('center_axis',(0.,0.,1.));
#13160=DIRECTION('ref_axis',(1.,0.,0.));
#13161=DIRECTION('',(0.,0.,1.));
#13162=DIRECTION('center_axis',(0.,0.,1.));
#13163=DIRECTION('ref_axis',(1.,0.,0.));
#13164=DIRECTION('center_axis',(0.,0.,1.));
#13165=DIRECTION('ref_axis',(1.,0.,0.));
#13166=DIRECTION('center_axis',(0.,0.,1.));
#13167=DIRECTION('ref_axis',(1.,0.,0.));
#13168=DIRECTION('',(0.,0.,1.));
#13169=DIRECTION('center_axis',(0.,0.,1.));
#13170=DIRECTION('ref_axis',(1.,0.,0.));
#13171=DIRECTION('center_axis',(0.,0.,-1.));
#13172=DIRECTION('ref_axis',(-1.,0.,0.));
#13173=DIRECTION('center_axis',(0.,0.,-1.));
#13174=DIRECTION('ref_axis',(-1.,0.,0.));
#13175=DIRECTION('',(0.,0.,-1.));
#13176=DIRECTION('center_axis',(0.,0.,1.));
#13177=DIRECTION('ref_axis',(-1.,0.,0.));
#13178=DIRECTION('center_axis',(0.,0.,1.));
#13179=DIRECTION('ref_axis',(1.,0.,0.));
#13180=DIRECTION('center_axis',(0.,0.,1.));
#13181=DIRECTION('ref_axis',(-1.,0.,0.));
#13182=DIRECTION('',(0.,0.,1.));
#13183=DIRECTION('center_axis',(0.,0.,1.));
#13184=DIRECTION('ref_axis',(-1.,0.,0.));
#13185=DIRECTION('center_axis',(0.,0.,1.));
#13186=DIRECTION('ref_axis',(1.,0.,0.));
#13187=DIRECTION('center_axis',(0.,0.,1.));
#13188=DIRECTION('ref_axis',(-1.,0.,0.));
#13189=DIRECTION('',(0.,0.,1.));
#13190=DIRECTION('center_axis',(0.,0.,1.));
#13191=DIRECTION('ref_axis',(-1.,0.,0.));
#13192=DIRECTION('center_axis',(0.,0.,1.));
#13193=DIRECTION('ref_axis',(1.,0.,0.));
#13194=DIRECTION('center_axis',(0.,0.,1.));
#13195=DIRECTION('ref_axis',(-1.,0.,0.));
#13196=DIRECTION('',(0.,0.,1.));
#13197=DIRECTION('center_axis',(0.,0.,1.));
#13198=DIRECTION('ref_axis',(1.,0.,0.));
#13199=DIRECTION('center_axis',(0.,0.,1.));
#13200=DIRECTION('ref_axis',(1.,0.,0.));
#13201=DIRECTION('center_axis',(0.,0.,1.));
#13202=DIRECTION('ref_axis',(-1.,0.,0.));
#13203=DIRECTION('',(0.,0.,1.));
#13204=DIRECTION('center_axis',(0.,0.,1.));
#13205=DIRECTION('ref_axis',(1.,0.,0.));
#13206=DIRECTION('center_axis',(0.,0.,1.));
#13207=DIRECTION('ref_axis',(1.,0.,0.));
#13208=DIRECTION('center_axis',(0.,0.,1.));
#13209=DIRECTION('ref_axis',(-1.,0.,0.));
#13210=DIRECTION('',(0.,0.,1.));
#13211=DIRECTION('center_axis',(0.,0.,1.));
#13212=DIRECTION('ref_axis',(1.,0.,0.));
#13213=DIRECTION('center_axis',(-1.,2.77555756156289E-16,0.));
#13214=DIRECTION('ref_axis',(-2.77555756156289E-16,-1.,0.));
#13215=DIRECTION('',(-3.31545529486744E-16,-1.,0.));
#13216=DIRECTION('',(0.,0.,1.));
#13217=DIRECTION('',(-4.78544407166016E-16,1.,0.));
#13218=DIRECTION('',(0.,0.,-1.));
#13219=DIRECTION('center_axis',(0.,-1.,0.));
#13220=DIRECTION('ref_axis',(0.,0.,-1.));
#13221=DIRECTION('',(1.,0.,0.));
#13222=DIRECTION('',(0.,0.,1.));
#13223=DIRECTION('',(-1.,0.,0.));
#13224=DIRECTION('',(0.,0.,-1.));
#13225=DIRECTION('center_axis',(1.,0.,0.));
#13226=DIRECTION('ref_axis',(0.,0.,-1.));
#13227=DIRECTION('',(0.,1.,0.));
#13228=DIRECTION('',(0.,0.,1.));
#13229=DIRECTION('',(0.,-1.,0.));
#13230=DIRECTION('',(0.,0.,-1.));
#13231=DIRECTION('center_axis',(0.,0.,-1.));
#13232=DIRECTION('ref_axis',(-1.,0.,0.));
#13233=DIRECTION('center_axis',(0.,0.,-1.));
#13234=DIRECTION('ref_axis',(-1.,0.,0.));
#13235=DIRECTION('center_axis',(0.,0.,1.));
#13236=DIRECTION('ref_axis',(1.,0.,0.));
#13237=DIRECTION('center_axis',(0.,0.,-1.));
#13238=DIRECTION('ref_axis',(-1.,0.,0.));
#13239=DIRECTION('center_axis',(0.,0.,-1.));
#13240=DIRECTION('ref_axis',(-1.,0.,0.));
#13241=DIRECTION('center_axis',(0.,0.,1.));
#13242=DIRECTION('ref_axis',(1.,0.,0.));
#13243=DIRECTION('center_axis',(0.,-1.,0.));
#13244=DIRECTION('ref_axis',(0.,0.,-1.));
#13245=DIRECTION('',(0.,0.,1.));
#13246=DIRECTION('',(1.,0.,0.));
#13247=DIRECTION('',(0.,0.,1.));
#13248=DIRECTION('',(1.,0.,0.));
#13249=DIRECTION('center_axis',(0.,0.,1.));
#13250=DIRECTION('ref_axis',(1.,0.,0.));
#13251=DIRECTION('center_axis',(0.,0.,1.));
#13252=DIRECTION('ref_axis',(-1.,0.,0.));
#13253=DIRECTION('',(0.,0.,1.));
#13254=DIRECTION('center_axis',(0.,0.,1.));
#13255=DIRECTION('ref_axis',(1.,0.,0.));
#13256=DIRECTION('center_axis',(-1.,-1.44560289664734E-16,0.));
#13257=DIRECTION('ref_axis',(1.44560289664734E-16,-1.,0.));
#13258=DIRECTION('',(1.44560289664734E-16,-1.,0.));
#13259=DIRECTION('',(0.,0.,1.));
#13260=DIRECTION('',(1.44560289664734E-16,-1.,0.));
#13261=DIRECTION('center_axis',(0.,0.,1.));
#13262=DIRECTION('ref_axis',(1.,0.,0.));
#13263=DIRECTION('center_axis',(0.,0.,1.));
#13264=DIRECTION('ref_axis',(-1.,1.15648231731787E-15,0.));
#13265=DIRECTION('',(0.,0.,1.));
#13266=DIRECTION('center_axis',(0.,0.,1.));
#13267=DIRECTION('ref_axis',(1.,0.,0.));
#13268=DIRECTION('center_axis',(0.,-1.,0.));
#13269=DIRECTION('ref_axis',(0.,0.,-1.));
#13270=DIRECTION('',(1.,0.,0.));
#13271=DIRECTION('',(0.,0.,1.));
#13272=DIRECTION('',(1.,0.,0.));
#13273=DIRECTION('center_axis',(0.,0.,1.));
#13274=DIRECTION('ref_axis',(1.,0.,0.));
#13275=DIRECTION('center_axis',(0.,0.,1.));
#13276=DIRECTION('ref_axis',(-1.,0.,0.));
#13277=DIRECTION('',(0.,0.,1.));
#13278=DIRECTION('center_axis',(0.,0.,1.));
#13279=DIRECTION('ref_axis',(1.,0.,0.));
#13280=DIRECTION('center_axis',(-1.,-1.44560289664734E-16,0.));
#13281=DIRECTION('ref_axis',(1.44560289664734E-16,-1.,0.));
#13282=DIRECTION('',(1.44560289664734E-16,-1.,0.));
#13283=DIRECTION('',(0.,0.,1.));
#13284=DIRECTION('',(1.44560289664734E-16,-1.,0.));
#13285=DIRECTION('center_axis',(0.,0.,1.));
#13286=DIRECTION('ref_axis',(1.,0.,0.));
#13287=DIRECTION('center_axis',(0.,0.,1.));
#13288=DIRECTION('ref_axis',(-1.,0.,0.));
#13289=DIRECTION('center_axis',(0.,0.,1.));
#13290=DIRECTION('ref_axis',(1.,0.,0.));
#13291=DIRECTION('center_axis',(-1.,-1.19636101791504E-16,0.));
#13292=DIRECTION('ref_axis',(1.19636101791504E-16,-1.,0.));
#13293=DIRECTION('',(0.,0.,-1.));
#13294=DIRECTION('',(0.,1.,0.));
#13295=DIRECTION('',(0.,0.,1.));
#13296=DIRECTION('',(1.19636101791504E-16,-1.,0.));
#13297=DIRECTION('center_axis',(-0.707106781186546,0.707106781186549,0.));
#13298=DIRECTION('ref_axis',(-0.707106781186549,-0.707106781186546,0.));
#13299=DIRECTION('',(0.,0.,-1.));
#13300=DIRECTION('',(0.707106781186549,0.707106781186546,0.));
#13301=DIRECTION('',(0.,0.,1.));
#13302=DIRECTION('',(-0.707106781186549,-0.707106781186546,0.));
#13303=DIRECTION('center_axis',(0.,-1.,0.));
#13304=DIRECTION('ref_axis',(0.,0.,-1.));
#13305=DIRECTION('',(0.,0.,-1.));
#13306=DIRECTION('',(-1.,6.42490176287706E-17,0.));
#13307=DIRECTION('',(0.,0.,1.));
#13308=DIRECTION('',(1.,0.,0.));
#13309=DIRECTION('center_axis',(1.,0.,0.));
#13310=DIRECTION('ref_axis',(0.,0.,-1.));
#13311=DIRECTION('',(0.,0.,-1.));
#13312=DIRECTION('',(0.,-1.,0.));
#13313=DIRECTION('',(0.,0.,1.));
#13314=DIRECTION('',(0.,1.,0.));
#13315=DIRECTION('center_axis',(0.707106781186547,-0.707106781186548,0.));
#13316=DIRECTION('ref_axis',(0.707106781186548,0.707106781186547,0.));
#13317=DIRECTION('',(0.,0.,-1.));
#13318=DIRECTION('',(-0.707106781186549,-0.707106781186546,0.));
#13319=DIRECTION('',(0.,0.,1.));
#13320=DIRECTION('',(0.707106781186548,0.707106781186547,0.));
#13321=DIRECTION('center_axis',(0.,0.,1.));
#13322=DIRECTION('ref_axis',(1.,0.,0.));
#13323=DIRECTION('center_axis',(0.,0.,-1.));
#13324=DIRECTION('ref_axis',(-1.,0.,0.));
#13325=DIRECTION('center_axis',(0.,0.,1.));
#13326=DIRECTION('ref_axis',(1.,0.,0.));
#13327=DIRECTION('center_axis',(0.,0.,-1.));
#13328=DIRECTION('ref_axis',(-1.,0.,0.));
#13329=DIRECTION('center_axis',(0.,0.,1.));
#13330=DIRECTION('ref_axis',(-1.,0.,0.));
#13331=DIRECTION('center_axis',(0.,0.,-1.));
#13332=DIRECTION('ref_axis',(1.,1.73472347597681E-15,0.));
#13333=DIRECTION('center_axis',(0.,0.,1.));
#13334=DIRECTION('ref_axis',(1.,0.,0.));
#13335=DIRECTION('center_axis',(0.,0.,-1.));
#13336=DIRECTION('ref_axis',(-1.,0.,0.));
#13337=DIRECTION('center_axis',(0.,0.,1.));
#13338=DIRECTION('ref_axis',(1.,0.,0.));
#13339=DIRECTION('center_axis',(0.,0.,1.));
#13340=DIRECTION('ref_axis',(1.,0.,0.));
#13341=DIRECTION('center_axis',(0.,0.,-1.));
#13342=DIRECTION('ref_axis',(-1.,0.,0.));
#13343=DIRECTION('center_axis',(0.,0.,1.));
#13344=DIRECTION('ref_axis',(1.,0.,0.));
#13345=DIRECTION('center_axis',(0.,0.,1.));
#13346=DIRECTION('ref_axis',(1.,0.,0.));
#13347=DIRECTION('center_axis',(0.,0.,-1.));
#13348=DIRECTION('ref_axis',(-1.,0.,0.));
#13349=DIRECTION('center_axis',(0.,0.,1.));
#13350=DIRECTION('ref_axis',(1.,0.,0.));
#13351=DIRECTION('center_axis',(0.,0.,1.));
#13352=DIRECTION('ref_axis',(1.,0.,0.));
#13353=DIRECTION('center_axis',(0.,0.,1.));
#13354=DIRECTION('ref_axis',(-1.,0.,0.));
#13355=DIRECTION('center_axis',(0.,0.,-1.));
#13356=DIRECTION('ref_axis',(1.,-2.08166817117217E-15,0.));
#13357=DIRECTION('center_axis',(0.,0.,1.));
#13358=DIRECTION('ref_axis',(1.,0.,0.));
#13359=DIRECTION('center_axis',(0.,0.,-1.));
#13360=DIRECTION('ref_axis',(-1.,0.,0.));
#13361=DIRECTION('center_axis',(0.,0.,-1.));
#13362=DIRECTION('ref_axis',(-1.,0.,0.));
#13363=DIRECTION('center_axis',(0.,0.,-1.));
#13364=DIRECTION('ref_axis',(-1.,0.,0.));
#13365=DIRECTION('center_axis',(0.,0.,-1.));
#13366=DIRECTION('ref_axis',(-1.,0.,0.));
#13367=DIRECTION('center_axis',(0.,0.,-1.));
#13368=DIRECTION('ref_axis',(-1.,0.,0.));
#13369=DIRECTION('axis',(0.,0.,1.));
#13370=DIRECTION('refdir',(1.,0.,0.));
#13371=DIRECTION('center_axis',(-1.,0.,0.));
#13372=DIRECTION('ref_axis',(0.,0.,1.));
#13373=DIRECTION('center_axis',(-1.,0.,0.));
#13374=DIRECTION('ref_axis',(0.,0.,1.));
#13375=DIRECTION('center_axis',(0.,-1.,1.22464679914735E-16));
#13376=DIRECTION('ref_axis',(0.,-1.22464679914735E-16,-1.));
#13377=DIRECTION('center_axis',(1.,0.,0.));
#13378=DIRECTION('ref_axis',(0.,0.,1.));
#13379=DIRECTION('center_axis',(1.,0.,0.));
#13380=DIRECTION('ref_axis',(0.,0.,-1.));
#13381=DIRECTION('center_axis',(1.,0.,0.));
#13382=DIRECTION('ref_axis',(0.,0.,-1.));
#13383=DIRECTION('center_axis',(1.,0.,0.));
#13384=DIRECTION('ref_axis',(0.,0.,-1.));
#13385=DIRECTION('center_axis',(0.,-1.,-1.22464679914735E-16));
#13386=DIRECTION('ref_axis',(0.,-1.22464679914735E-16,1.));
#13387=DIRECTION('center_axis',(-1.,0.,0.));
#13388=DIRECTION('ref_axis',(0.,0.,-1.));
#13389=DIRECTION('center_axis',(-1.,0.,0.));
#13390=DIRECTION('ref_axis',(0.,0.,1.));
#13391=DIRECTION('center_axis',(-1.,0.,0.));
#13392=DIRECTION('ref_axis',(0.,0.,1.));
#13393=DIRECTION('center_axis',(0.,-1.,1.22464679914735E-16));
#13394=DIRECTION('ref_axis',(0.,-1.22464679914735E-16,-1.));
#13395=DIRECTION('center_axis',(1.,0.,0.));
#13396=DIRECTION('ref_axis',(0.,0.,1.));
#13397=DIRECTION('center_axis',(1.,0.,0.));
#13398=DIRECTION('ref_axis',(0.,0.,-1.));
#13399=DIRECTION('center_axis',(1.,0.,0.));
#13400=DIRECTION('ref_axis',(0.,0.,-1.));
#13401=DIRECTION('center_axis',(1.,0.,0.));
#13402=DIRECTION('ref_axis',(0.,0.,-1.));
#13403=DIRECTION('center_axis',(0.,-1.,-1.22464679914735E-16));
#13404=DIRECTION('ref_axis',(0.,-1.22464679914735E-16,1.));
#13405=DIRECTION('center_axis',(-1.,0.,0.));
#13406=DIRECTION('ref_axis',(0.,0.,-1.));
#13407=DIRECTION('center_axis',(-1.,0.,0.));
#13408=DIRECTION('ref_axis',(0.,0.,1.));
#13409=DIRECTION('',(1.,0.,0.));
#13410=DIRECTION('center_axis',(-1.,0.,0.));
#13411=DIRECTION('ref_axis',(0.,0.,1.));
#13412=DIRECTION('center_axis',(-1.,0.,0.));
#13413=DIRECTION('ref_axis',(0.,0.,1.));
#13414=DIRECTION('',(1.,0.,0.));
#13415=DIRECTION('center_axis',(-1.,0.,0.));
#13416=DIRECTION('ref_axis',(0.,0.,1.));
#13417=DIRECTION('center_axis',(-1.,0.,0.));
#13418=DIRECTION('ref_axis',(0.,0.,1.));
#13419=DIRECTION('',(1.,0.,0.));
#13420=DIRECTION('center_axis',(-1.,0.,0.));
#13421=DIRECTION('ref_axis',(0.,0.,1.));
#13422=DIRECTION('center_axis',(1.,0.,0.));
#13423=DIRECTION('ref_axis',(0.,0.,-1.));
#13424=DIRECTION('center_axis',(-1.,0.,0.));
#13425=DIRECTION('ref_axis',(0.,0.,1.));
#13426=DIRECTION('center_axis',(-1.,0.,0.));
#13427=DIRECTION('ref_axis',(0.,0.,1.));
#13428=DIRECTION('',(0.,1.,0.));
#13429=DIRECTION('center_axis',(-1.,0.,0.));
#13430=DIRECTION('ref_axis',(0.,0.,1.));
#13431=DIRECTION('',(0.,1.,-4.7819200545485E-16));
#13432=DIRECTION('center_axis',(1.,0.,0.));
#13433=DIRECTION('ref_axis',(0.,0.,-1.));
#13434=DIRECTION('center_axis',(-1.,0.,0.));
#13435=DIRECTION('ref_axis',(0.,0.,1.));
#13436=DIRECTION('',(0.,1.,0.));
#13437=DIRECTION('center_axis',(-1.,0.,0.));
#13438=DIRECTION('ref_axis',(0.,0.,1.));
#13439=DIRECTION('',(0.,1.,-4.7819200545485E-16));
#13440=DIRECTION('center_axis',(0.,0.,1.));
#13441=DIRECTION('ref_axis',(1.,0.,0.));
#13442=DIRECTION('',(-1.,0.,0.));
#13443=DIRECTION('',(-1.,0.,0.));
#13444=DIRECTION('center_axis',(-1.,0.,0.));
#13445=DIRECTION('ref_axis',(0.,0.,1.));
#13446=DIRECTION('',(-1.,0.,0.));
#13447=DIRECTION('center_axis',(0.,4.7819200545485E-16,1.));
#13448=DIRECTION('ref_axis',(0.,-1.,4.7819200545485E-16));
#13449=DIRECTION('',(-1.,0.,0.));
#13450=DIRECTION('center_axis',(-1.,0.,0.));
#13451=DIRECTION('ref_axis',(0.,0.,1.));
#13452=DIRECTION('axis',(0.,0.,1.));
#13453=DIRECTION('refdir',(1.,0.,0.));
#13454=DIRECTION('center_axis',(-1.,0.,0.));
#13455=DIRECTION('ref_axis',(0.,0.,1.));
#13456=DIRECTION('center_axis',(-1.,0.,0.));
#13457=DIRECTION('ref_axis',(0.,0.,1.));
#13458=DIRECTION('',(-1.,0.,0.));
#13459=DIRECTION('center_axis',(-1.,0.,0.));
#13460=DIRECTION('ref_axis',(0.,0.,1.));
#13461=DIRECTION('center_axis',(-1.,0.,0.));
#13462=DIRECTION('ref_axis',(0.,0.,1.));
#13463=DIRECTION('center_axis',(-1.,0.,0.));
#13464=DIRECTION('ref_axis',(0.,0.,1.));
#13465=DIRECTION('center_axis',(0.,-1.,1.22464679914735E-16));
#13466=DIRECTION('ref_axis',(0.,-1.22464679914735E-16,-1.));
#13467=DIRECTION('center_axis',(1.,0.,0.));
#13468=DIRECTION('ref_axis',(0.,0.,1.));
#13469=DIRECTION('center_axis',(1.,0.,0.));
#13470=DIRECTION('ref_axis',(0.,0.,-1.));
#13471=DIRECTION('center_axis',(1.,0.,0.));
#13472=DIRECTION('ref_axis',(0.,0.,-1.));
#13473=DIRECTION('center_axis',(1.,0.,0.));
#13474=DIRECTION('ref_axis',(0.,0.,-1.));
#13475=DIRECTION('center_axis',(0.,-1.,-1.22464679914735E-16));
#13476=DIRECTION('ref_axis',(0.,-1.22464679914735E-16,1.));
#13477=DIRECTION('center_axis',(-1.,0.,0.));
#13478=DIRECTION('ref_axis',(0.,0.,-1.));
#13479=DIRECTION('center_axis',(-1.,0.,0.));
#13480=DIRECTION('ref_axis',(0.,0.,1.));
#13481=DIRECTION('center_axis',(-1.,0.,0.));
#13482=DIRECTION('ref_axis',(0.,0.,1.));
#13483=DIRECTION('center_axis',(0.,-1.,1.22464679914735E-16));
#13484=DIRECTION('ref_axis',(0.,-1.22464679914735E-16,-1.));
#13485=DIRECTION('center_axis',(1.,0.,0.));
#13486=DIRECTION('ref_axis',(0.,0.,1.));
#13487=DIRECTION('center_axis',(1.,0.,0.));
#13488=DIRECTION('ref_axis',(0.,0.,-1.));
#13489=DIRECTION('center_axis',(1.,0.,0.));
#13490=DIRECTION('ref_axis',(0.,0.,-1.));
#13491=DIRECTION('center_axis',(1.,0.,0.));
#13492=DIRECTION('ref_axis',(0.,0.,-1.));
#13493=DIRECTION('center_axis',(0.,-1.,-1.22464679914735E-16));
#13494=DIRECTION('ref_axis',(0.,-1.22464679914735E-16,1.));
#13495=DIRECTION('center_axis',(-1.,0.,0.));
#13496=DIRECTION('ref_axis',(0.,0.,-1.));
#13497=DIRECTION('center_axis',(-1.,0.,0.));
#13498=DIRECTION('ref_axis',(0.,0.,1.));
#13499=DIRECTION('',(1.,0.,0.));
#13500=DIRECTION('center_axis',(-1.,0.,0.));
#13501=DIRECTION('ref_axis',(0.,0.,1.));
#13502=DIRECTION('center_axis',(-1.,0.,0.));
#13503=DIRECTION('ref_axis',(0.,0.,1.));
#13504=DIRECTION('',(1.,0.,0.));
#13505=DIRECTION('center_axis',(-1.,0.,0.));
#13506=DIRECTION('ref_axis',(0.,0.,1.));
#13507=DIRECTION('center_axis',(-1.,0.,0.));
#13508=DIRECTION('ref_axis',(0.,0.,1.));
#13509=DIRECTION('',(1.,0.,0.));
#13510=DIRECTION('center_axis',(-1.,0.,0.));
#13511=DIRECTION('ref_axis',(0.,0.,1.));
#13512=DIRECTION('center_axis',(1.,0.,0.));
#13513=DIRECTION('ref_axis',(0.,0.,-1.));
#13514=DIRECTION('center_axis',(-1.,0.,0.));
#13515=DIRECTION('ref_axis',(0.,0.,1.));
#13516=DIRECTION('center_axis',(1.,0.,0.));
#13517=DIRECTION('ref_axis',(0.,0.,-1.));
#13518=DIRECTION('axis',(0.,0.,1.));
#13519=DIRECTION('refdir',(1.,0.,0.));
#13520=DIRECTION('center_axis',(0.,0.,-1.));
#13521=DIRECTION('ref_axis',(-1.,0.,0.));
#13522=DIRECTION('center_axis',(0.,0.,-1.));
#13523=DIRECTION('ref_axis',(-1.,0.,0.));
#13524=DIRECTION('center_axis',(0.,-1.,0.));
#13525=DIRECTION('ref_axis',(1.,0.,0.));
#13526=DIRECTION('center_axis',(0.,0.,1.));
#13527=DIRECTION('ref_axis',(-1.,0.,0.));
#13528=DIRECTION('center_axis',(0.,0.,1.));
#13529=DIRECTION('ref_axis',(-1.,0.,0.));
#13530=DIRECTION('center_axis',(0.,0.,1.));
#13531=DIRECTION('ref_axis',(1.,0.,0.));
#13532=DIRECTION('center_axis',(0.,0.,-1.));
#13533=DIRECTION('ref_axis',(1.,0.,0.));
#13534=DIRECTION('',(0.,0.,-1.));
#13535=DIRECTION('center_axis',(0.,0.,-1.));
#13536=DIRECTION('ref_axis',(-1.,0.,0.));
#13537=DIRECTION('center_axis',(0.,0.,-1.));
#13538=DIRECTION('ref_axis',(1.,0.,0.));
#13539=DIRECTION('',(0.,0.,-1.));
#13540=DIRECTION('center_axis',(0.,0.,-1.));
#13541=DIRECTION('ref_axis',(-1.,0.,0.));
#13542=DIRECTION('center_axis',(0.,0.,-1.));
#13543=DIRECTION('ref_axis',(-1.,0.,0.));
#13544=DIRECTION('center_axis',(0.,0.,-1.));
#13545=DIRECTION('ref_axis',(1.,0.,0.));
#13546=DIRECTION('',(0.,0.,-1.));
#13547=DIRECTION('center_axis',(0.,0.,-1.));
#13548=DIRECTION('ref_axis',(-1.,0.,0.));
#13549=DIRECTION('center_axis',(0.,0.,-1.));
#13550=DIRECTION('ref_axis',(-1.,0.,0.));
#13551=DIRECTION('center_axis',(0.,0.,-1.));
#13552=DIRECTION('ref_axis',(1.,0.,0.));
#13553=DIRECTION('',(0.,0.,-1.));
#13554=DIRECTION('center_axis',(0.,0.,-1.));
#13555=DIRECTION('ref_axis',(-1.,0.,0.));
#13556=DIRECTION('center_axis',(0.,0.,-1.));
#13557=DIRECTION('ref_axis',(-1.,0.,0.));
#13558=DIRECTION('center_axis',(0.,0.,-1.));
#13559=DIRECTION('ref_axis',(1.,0.,0.));
#13560=DIRECTION('',(0.,0.,-1.));
#13561=DIRECTION('center_axis',(0.,0.,-1.));
#13562=DIRECTION('ref_axis',(-1.,0.,0.));
#13563=DIRECTION('center_axis',(0.,0.,1.));
#13564=DIRECTION('ref_axis',(1.,0.,0.));
#13565=DIRECTION('center_axis',(0.,0.,-1.));
#13566=DIRECTION('ref_axis',(1.,0.,0.));
#13567=DIRECTION('',(0.,0.,1.));
#13568=DIRECTION('center_axis',(0.,0.,1.));
#13569=DIRECTION('ref_axis',(1.,0.,0.));
#13570=DIRECTION('center_axis',(0.,0.,1.));
#13571=DIRECTION('ref_axis',(1.,0.,0.));
#13572=DIRECTION('center_axis',(0.,0.,-1.));
#13573=DIRECTION('ref_axis',(1.,0.,0.));
#13574=DIRECTION('',(0.,0.,-1.));
#13575=DIRECTION('center_axis',(0.,0.,-1.));
#13576=DIRECTION('ref_axis',(-1.,0.,0.));
#13577=DIRECTION('',(0.,0.,1.));
#13578=DIRECTION('center_axis',(0.,0.,-1.));
#13579=DIRECTION('ref_axis',(-1.,0.,0.));
#13580=DIRECTION('',(0.,0.,-1.));
#13581=DIRECTION('center_axis',(0.,0.,-1.));
#13582=DIRECTION('ref_axis',(-1.,0.,0.));
#13583=DIRECTION('',(0.,0.,1.));
#13584=DIRECTION('center_axis',(0.,0.,-1.));
#13585=DIRECTION('ref_axis',(-1.,0.,0.));
#13586=DIRECTION('',(0.,0.,-1.));
#13587=DIRECTION('center_axis',(0.,0.,-1.));
#13588=DIRECTION('ref_axis',(-1.,0.,0.));
#13589=DIRECTION('center_axis',(1.,3.08395284618099E-16,0.));
#13590=DIRECTION('ref_axis',(0.,1.,0.));
#13591=DIRECTION('center_axis',(-1.,0.,0.));
#13592=DIRECTION('ref_axis',(0.,1.,0.));
#13593=DIRECTION('center_axis',(1.,0.,0.));
#13594=DIRECTION('ref_axis',(0.,1.,0.));
#13595=DIRECTION('center_axis',(-1.,0.,0.));
#13596=DIRECTION('ref_axis',(0.,-1.,0.));
#13597=DIRECTION('center_axis',(-1.,-8.83324975243572E-46,5.21932234251264E-31));
#13598=DIRECTION('ref_axis',(-7.64335950198467E-61,1.,1.69241314729438E-15));
#13599=DIRECTION('',(-1.,-3.08395284618099E-16,0.));
#13600=DIRECTION('center_axis',(1.,0.,0.));
#13601=DIRECTION('ref_axis',(0.,1.,0.));
#13602=DIRECTION('',(-1.,-3.08395284618099E-16,0.));
#13603=DIRECTION('center_axis',(-1.,0.,0.));
#13604=DIRECTION('ref_axis',(0.,-1.,0.));
#13605=DIRECTION('center_axis',(1.,0.,0.));
#13606=DIRECTION('ref_axis',(0.,1.,0.));
#13607=DIRECTION('',(-1.,-3.08395284618099E-16,0.));
#13608=DIRECTION('center_axis',(1.,0.,0.));
#13609=DIRECTION('ref_axis',(0.,1.,0.));
#13610=DIRECTION('center_axis',(1.,0.,0.));
#13611=DIRECTION('ref_axis',(0.,1.,0.));
#13612=DIRECTION('',(1.,3.08395284618099E-16,0.));
#13613=DIRECTION('center_axis',(0.,0.,-1.));
#13614=DIRECTION('ref_axis',(-1.,0.,0.));
#13615=DIRECTION('center_axis',(0.,0.,1.));
#13616=DIRECTION('ref_axis',(1.,0.,0.));
#13617=DIRECTION('',(0.,0.,1.));
#13618=DIRECTION('center_axis',(0.,0.,-1.));
#13619=DIRECTION('ref_axis',(-1.,0.,0.));
#13620=DIRECTION('',(0.,0.,-1.));
#13621=DIRECTION('center_axis',(0.,0.,-1.));
#13622=DIRECTION('ref_axis',(1.,6.30808536718839E-16,0.));
#13623=DIRECTION('',(0.,0.,1.));
#13624=DIRECTION('center_axis',(0.,0.,-1.));
#13625=DIRECTION('ref_axis',(-1.,0.,0.));
#13626=DIRECTION('',(0.,0.,-1.));
#13627=DIRECTION('center_axis',(0.,0.,-1.));
#13628=DIRECTION('ref_axis',(1.,6.30808536718839E-16,0.));
#13629=DIRECTION('',(0.,0.,1.));
#13630=DIRECTION('center_axis',(0.,0.,-1.));
#13631=DIRECTION('ref_axis',(-1.,0.,0.));
#13632=DIRECTION('center_axis',(0.,0.,1.));
#13633=DIRECTION('ref_axis',(1.,0.,0.));
#13634=DIRECTION('',(-3.08395284618099E-16,1.,0.));
#13635=DIRECTION('',(1.,0.,0.));
#13636=DIRECTION('center_axis',(0.,0.,1.));
#13637=DIRECTION('ref_axis',(-1.,0.,0.));
#13638=DIRECTION('',(0.,-1.,0.));
#13639=DIRECTION('center_axis',(0.,0.,1.));
#13640=DIRECTION('ref_axis',(1.,0.,0.));
#13641=DIRECTION('',(-1.,0.,0.));
#13642=DIRECTION('',(-3.08395284618099E-16,1.,0.));
#13643=DIRECTION('',(-1.,-3.08395284618099E-16,0.));
#13644=DIRECTION('',(3.09492820192543E-16,-1.,0.));
#13645=DIRECTION('center_axis',(-1.,0.,0.));
#13646=DIRECTION('ref_axis',(0.,0.,1.));
#13647=DIRECTION('',(0.,-1.,0.));
#13648=DIRECTION('',(0.,0.,1.));
#13649=DIRECTION('',(0.,0.,1.));
#13650=DIRECTION('',(0.,0.,1.));
#13651=DIRECTION('',(0.,-1.,0.));
#13652=DIRECTION('',(0.,0.,-1.));
#13653=DIRECTION('',(0.,1.,-3.46944695195362E-16));
#13654=DIRECTION('center_axis',(0.,0.,1.));
#13655=DIRECTION('ref_axis',(1.,0.,0.));
#13656=DIRECTION('',(1.,0.,0.));
#13657=DIRECTION('',(-1.,0.,0.));
#13658=DIRECTION('center_axis',(1.,2.93307512767319E-47,9.51076515746783E-32));
#13659=DIRECTION('ref_axis',(8.86148785842978E-64,1.,-3.08395284618099E-16));
#13660=DIRECTION('center_axis',(1.,0.,0.));
#13661=DIRECTION('ref_axis',(0.,1.,0.));
#13662=DIRECTION('',(-3.01691039300315E-16,1.,0.));
#13663=DIRECTION('',(4.96586290813306E-16,-1.,0.));
#13664=DIRECTION('center_axis',(1.,0.,0.));
#13665=DIRECTION('ref_axis',(0.,1.,0.));
#13666=DIRECTION('',(-5.41424068523692E-16,1.,0.));
#13667=DIRECTION('center_axis',(-1.,0.,0.));
#13668=DIRECTION('ref_axis',(0.,0.998520612789804,-0.0543744961712152));
#13669=DIRECTION('center_axis',(1.,0.,0.));
#13670=DIRECTION('ref_axis',(0.,1.,0.));
#13671=DIRECTION('center_axis',(1.,0.,0.));
#13672=DIRECTION('ref_axis',(0.,1.,0.));
#13673=DIRECTION('',(1.,3.08395284618099E-16,0.));
#13674=DIRECTION('center_axis',(1.,2.93307512767319E-47,9.51076515746783E-32));
#13675=DIRECTION('ref_axis',(8.86148785842978E-64,1.,-3.08395284618099E-16));
#13676=DIRECTION('',(0.,0.,1.));
#13677=DIRECTION('center_axis',(1.,2.93307512767319E-47,9.51076515746783E-32));
#13678=DIRECTION('ref_axis',(8.86148785842978E-64,1.,-3.08395284618099E-16));
#13679=DIRECTION('',(0.,0.,1.));
#13680=DIRECTION('',(-3.08395284618099E-16,1.,0.));
#13681=DIRECTION('',(0.,0.,1.));
#13682=DIRECTION('',(-3.01691039300315E-16,1.,0.));
#13683=DIRECTION('center_axis',(1.,2.93307512767319E-47,9.51076515746783E-32));
#13684=DIRECTION('ref_axis',(8.86148785842978E-64,1.,-3.08395284618099E-16));
#13685=DIRECTION('',(0.,0.,1.));
#13686=DIRECTION('center_axis',(0.,-1.,0.));
#13687=DIRECTION('ref_axis',(0.,0.,-1.));
#13688=DIRECTION('',(1.,0.,0.));
#13689=DIRECTION('',(0.,0.,1.));
#13690=DIRECTION('center_axis',(0.,0.,1.));
#13691=DIRECTION('ref_axis',(1.,0.,0.));
#13692=DIRECTION('center_axis',(0.,0.,1.));
#13693=DIRECTION('ref_axis',(-1.,0.,0.));
#13694=DIRECTION('center_axis',(0.,0.,1.));
#13695=DIRECTION('ref_axis',(1.,0.,0.));
#13696=DIRECTION('center_axis',(0.,0.,1.));
#13697=DIRECTION('ref_axis',(1.,0.,0.));
#13698=DIRECTION('',(0.,0.,1.));
#13699=DIRECTION('center_axis',(0.,1.,0.));
#13700=DIRECTION('ref_axis',(1.,0.,0.));
#13701=DIRECTION('',(-1.,0.,0.));
#13702=DIRECTION('center_axis',(0.,0.,1.));
#13703=DIRECTION('ref_axis',(1.,0.,0.));
#13704=DIRECTION('center_axis',(0.,0.,-1.));
#13705=DIRECTION('ref_axis',(0.,-1.,0.));
#13706=DIRECTION('center_axis',(-1.,0.,0.));
#13707=DIRECTION('ref_axis',(0.,0.999304019410872,-0.0373025037936587));
#13708=DIRECTION('',(-1.,-3.08395284618099E-16,0.));
#13709=DIRECTION('',(-1.,-3.08395284618099E-16,0.));
#13710=DIRECTION('center_axis',(0.,0.,-1.));
#13711=DIRECTION('ref_axis',(0.,-1.,0.));
#13712=DIRECTION('',(-3.08395284618099E-16,1.,0.));
#13713=DIRECTION('center_axis',(0.,0.,1.));
#13714=DIRECTION('ref_axis',(1.,0.,0.));
#13715=DIRECTION('',(3.08395284618099E-16,-1.,0.));
#13716=DIRECTION('center_axis',(1.,2.93307512767319E-47,9.51076515746783E-32));
#13717=DIRECTION('ref_axis',(8.86148785842978E-64,1.,-3.08395284618099E-16));
#13718=DIRECTION('center_axis',(1.,0.,0.));
#13719=DIRECTION('ref_axis',(0.,1.,0.));
#13720=DIRECTION('',(-3.08395284618099E-16,1.,0.));
#13721=DIRECTION('',(3.08395284618099E-16,-1.,0.));
#13722=DIRECTION('center_axis',(0.,1.,0.));
#13723=DIRECTION('ref_axis',(-1.,0.,0.));
#13724=DIRECTION('center_axis',(1.,3.08395284618099E-16,0.));
#13725=DIRECTION('ref_axis',(0.,-0.999304019410872,-0.0373025037936637));
#13726=DIRECTION('center_axis',(0.,-1.,0.));
#13727=DIRECTION('ref_axis',(1.,0.,0.));
#13728=DIRECTION('center_axis',(0.,0.,-1.));
#13729=DIRECTION('ref_axis',(0.,-1.,0.));
#13730=DIRECTION('',(1.,0.,0.));
#13731=DIRECTION('',(-1.,0.,0.));
#13732=DIRECTION('center_axis',(0.,0.,-1.));
#13733=DIRECTION('ref_axis',(0.,-1.,0.));
#13734=DIRECTION('',(-1.,0.,0.));
#13735=DIRECTION('center_axis',(0.,-1.,0.));
#13736=DIRECTION('ref_axis',(0.,0.,-1.));
#13737=DIRECTION('center_axis',(0.,0.,-1.));
#13738=DIRECTION('ref_axis',(0.,-1.,0.));
#13739=DIRECTION('',(1.,0.,0.));
#13740=DIRECTION('center_axis',(0.,1.,0.));
#13741=DIRECTION('ref_axis',(1.,0.,0.));
#13742=DIRECTION('center_axis',(0.,1.,0.));
#13743=DIRECTION('ref_axis',(1.,0.,0.));
#13744=DIRECTION('',(-1.,0.,0.));
#13745=DIRECTION('center_axis',(0.,0.,1.));
#13746=DIRECTION('ref_axis',(1.,0.,0.));
#13747=DIRECTION('center_axis',(0.,-1.,0.));
#13748=DIRECTION('ref_axis',(0.,0.,-1.));
#13749=DIRECTION('',(1.,0.,0.));
#13750=DIRECTION('center_axis',(0.,0.,1.));
#13751=DIRECTION('ref_axis',(1.,0.,0.));
#13752=DIRECTION('center_axis',(0.,0.,1.));
#13753=DIRECTION('ref_axis',(1.,0.,0.));
#13754=DIRECTION('',(1.,0.,0.));
#13755=DIRECTION('',(0.,-1.,0.));
#13756=DIRECTION('',(1.,0.,0.));
#13757=DIRECTION('center_axis',(0.,1.,0.));
#13758=DIRECTION('ref_axis',(1.,0.,0.));
#13759=DIRECTION('',(1.,0.,0.));
#13760=DIRECTION('',(0.,0.,1.));
#13761=DIRECTION('center_axis',(0.,-3.46944695195362E-16,-1.));
#13762=DIRECTION('ref_axis',(0.,-1.,3.46944695195362E-16));
#13763=DIRECTION('',(1.,0.,0.));
#13764=DIRECTION('',(0.,1.,-3.46944695195362E-16));
#13765=DIRECTION('center_axis',(0.,-1.,0.));
#13766=DIRECTION('ref_axis',(0.,0.,-1.));
#13767=DIRECTION('',(0.,0.,-1.));
#13768=DIRECTION('center_axis',(-1.,0.,0.));
#13769=DIRECTION('ref_axis',(0.,0.,1.));
#13770=DIRECTION('center_axis',(0.,0.,-1.));
#13771=DIRECTION('ref_axis',(0.,-1.,0.));
#13772=DIRECTION('axis',(0.,0.,1.));
#13773=DIRECTION('refdir',(1.,0.,0.));
#13774=DIRECTION('center_axis',(0.,0.,-1.));
#13775=DIRECTION('ref_axis',(-1.,0.,0.));
#13776=DIRECTION('center_axis',(0.,0.,1.));
#13777=DIRECTION('ref_axis',(1.,0.,0.));
#13778=DIRECTION('',(0.,0.,-1.));
#13779=DIRECTION('center_axis',(0.,0.,1.));
#13780=DIRECTION('ref_axis',(1.,0.,0.));
#13781=DIRECTION('',(0.,0.,-1.));
#13782=DIRECTION('center_axis',(0.,0.,-1.));
#13783=DIRECTION('ref_axis',(-1.,0.,0.));
#13784=DIRECTION('center_axis',(0.,0.,1.));
#13785=DIRECTION('ref_axis',(1.,0.,0.));
#13786=DIRECTION('',(0.,0.,-1.));
#13787=DIRECTION('center_axis',(0.,0.,1.));
#13788=DIRECTION('ref_axis',(1.,0.,0.));
#13789=DIRECTION('',(0.,0.,-1.));
#13790=DIRECTION('center_axis',(0.,0.,1.));
#13791=DIRECTION('ref_axis',(1.,0.,0.));
#13792=DIRECTION('',(0.995540072322484,-0.0943396226415094,0.));
#13793=DIRECTION('center_axis',(0.,0.,1.));
#13794=DIRECTION('ref_axis',(1.,0.,0.));
#13795=DIRECTION('',(-0.995540072322484,-0.0943396226415094,0.));
#13796=DIRECTION('',(0.995540072322484,-0.0943396226415095,0.));
#13797=DIRECTION('',(-0.995540072322484,-0.0943396226415095,0.));
#13798=DIRECTION('center_axis',(0.,0.,1.));
#13799=DIRECTION('ref_axis',(1.,0.,0.));
#13800=DIRECTION('center_axis',(0.,0.,1.));
#13801=DIRECTION('ref_axis',(1.,0.,0.));
#13802=DIRECTION('',(-0.995540072322484,-0.0943396226415094,0.));
#13803=DIRECTION('center_axis',(0.,0.,1.));
#13804=DIRECTION('ref_axis',(1.,0.,0.));
#13805=DIRECTION('',(0.995540072322484,-0.0943396226415094,0.));
#13806=DIRECTION('',(0.995540072322484,-0.0943396226415095,0.));
#13807=DIRECTION('center_axis',(0.,0.,1.));
#13808=DIRECTION('ref_axis',(1.,0.,0.));
#13809=DIRECTION('',(-0.995540072322484,-0.0943396226415095,0.));
#13810=DIRECTION('center_axis',(0.0943396226415094,0.995540072322485,0.));
#13811=DIRECTION('ref_axis',(-0.995540072322485,0.0943396226415094,0.));
#13812=DIRECTION('',(0.,0.,-1.));
#13813=DIRECTION('center_axis',(0.,0.,-1.));
#13814=DIRECTION('ref_axis',(1.,-3.21624529935327E-16,0.));
#13815=DIRECTION('',(0.,0.,-1.));
#13816=DIRECTION('center_axis',(0.0943396226415095,-0.995540072322485,0.));
#13817=DIRECTION('ref_axis',(0.995540072322485,0.0943396226415095,0.));
#13818=DIRECTION('center_axis',(0.0943396226415095,0.995540072322485,0.));
#13819=DIRECTION('ref_axis',(-0.995540072322485,0.0943396226415095,0.));
#13820=DIRECTION('',(0.,0.,-1.));
#13821=DIRECTION('center_axis',(0.,0.,-1.));
#13822=DIRECTION('ref_axis',(1.,1.22464679914735E-16,0.));
#13823=DIRECTION('',(0.,0.,-1.));
#13824=DIRECTION('center_axis',(0.0943396226415095,-0.995540072322485,0.));
#13825=DIRECTION('ref_axis',(0.995540072322485,0.0943396226415095,0.));
#13826=DIRECTION('axis',(0.,0.,1.));
#13827=DIRECTION('refdir',(1.,0.,0.));
#13828=DIRECTION('center_axis',(0.,0.,-1.));
#13829=DIRECTION('ref_axis',(-1.,0.,0.));
#13830=DIRECTION('center_axis',(0.,0.,1.));
#13831=DIRECTION('ref_axis',(1.,0.,0.));
#13832=DIRECTION('',(0.,0.,-1.));
#13833=DIRECTION('center_axis',(0.,0.,1.));
#13834=DIRECTION('ref_axis',(1.,0.,0.));
#13835=DIRECTION('',(0.,0.,-1.));
#13836=DIRECTION('center_axis',(0.,0.,-1.));
#13837=DIRECTION('ref_axis',(-1.,0.,0.));
#13838=DIRECTION('center_axis',(0.,0.,1.));
#13839=DIRECTION('ref_axis',(1.,0.,0.));
#13840=DIRECTION('',(0.,0.,-1.));
#13841=DIRECTION('center_axis',(0.,0.,1.));
#13842=DIRECTION('ref_axis',(1.,0.,0.));
#13843=DIRECTION('',(0.,0.,-1.));
#13844=DIRECTION('center_axis',(0.,0.,1.));
#13845=DIRECTION('ref_axis',(1.,0.,0.));
#13846=DIRECTION('',(0.977572309327645,-0.210600047568408,0.));
#13847=DIRECTION('',(1.,1.18563999046388E-16,0.));
#13848=DIRECTION('',(0.980975643997698,0.194130847325459,0.));
#13849=DIRECTION('center_axis',(0.,0.,1.));
#13850=DIRECTION('ref_axis',(-1.,0.,0.));
#13851=DIRECTION('',(-1.,-1.23321574121574E-16,0.));
#13852=DIRECTION('',(0.977572309327645,-0.210600047568409,0.));
#13853=DIRECTION('',(-1.,-1.23321574121574E-16,0.));
#13854=DIRECTION('center_axis',(0.,0.,1.));
#13855=DIRECTION('ref_axis',(-1.,0.,0.));
#13856=DIRECTION('',(0.980975643997698,0.194130847325459,0.));
#13857=DIRECTION('',(1.,1.09561482693272E-16,0.));
#13858=DIRECTION('center_axis',(0.,0.,1.));
#13859=DIRECTION('ref_axis',(1.,0.,0.));
#13860=DIRECTION('',(-1.,-1.23321574121574E-16,0.));
#13861=DIRECTION('center_axis',(0.,0.,1.));
#13862=DIRECTION('ref_axis',(-1.,0.,0.));
#13863=DIRECTION('',(0.980975643997698,0.194130847325459,0.));
#13864=DIRECTION('',(1.,1.18563999046388E-16,0.));
#13865=DIRECTION('',(0.977572309327645,-0.210600047568408,0.));
#13866=DIRECTION('',(0.977572309327645,-0.210600047568409,0.));
#13867=DIRECTION('',(1.,1.09561482693272E-16,0.));
#13868=DIRECTION('',(0.980975643997698,0.194130847325459,0.));
#13869=DIRECTION('center_axis',(0.,0.,1.));
#13870=DIRECTION('ref_axis',(-1.,0.,0.));
#13871=DIRECTION('',(-1.,-1.23321574121574E-16,0.));
#13872=DIRECTION('center_axis',(0.210600047568408,0.977572309327645,0.));
#13873=DIRECTION('ref_axis',(-0.977572309327645,0.210600047568408,0.));
#13874=DIRECTION('',(0.,0.,-1.));
#13875=DIRECTION('center_axis',(-1.18563999046388E-16,1.,0.));
#13876=DIRECTION('ref_axis',(-1.,-1.18563999046388E-16,0.));
#13877=DIRECTION('',(0.,0.,-1.));
#13878=DIRECTION('center_axis',(-0.194130847325459,0.980975643997699,0.));
#13879=DIRECTION('ref_axis',(-0.980975643997699,-0.19413084732546,0.));
#13880=DIRECTION('',(0.,0.,-1.));
#13881=DIRECTION('center_axis',(0.,0.,-1.));
#13882=DIRECTION('ref_axis',(0.995232546693912,0.0975303952680951,0.));
#13883=DIRECTION('',(0.,0.,-1.));
#13884=DIRECTION('center_axis',(1.23321574121574E-16,-1.,0.));
#13885=DIRECTION('ref_axis',(1.,1.23321574121574E-16,0.));
#13886=DIRECTION('center_axis',(0.210600047568409,0.977572309327645,0.));
#13887=DIRECTION('ref_axis',(-0.977572309327645,0.210600047568409,0.));
#13888=DIRECTION('',(0.,0.,-1.));
#13889=DIRECTION('center_axis',(-1.09561482693272E-16,1.,0.));
#13890=DIRECTION('ref_axis',(-1.,-1.09561482693272E-16,0.));
#13891=DIRECTION('',(0.,0.,-1.));
#13892=DIRECTION('center_axis',(-0.194130847325459,0.980975643997699,0.));
#13893=DIRECTION('ref_axis',(-0.980975643997699,-0.194130847325459,0.));
#13894=DIRECTION('',(0.,0.,-1.));
#13895=DIRECTION('center_axis',(0.,0.,-1.));
#13896=DIRECTION('ref_axis',(0.995232546693912,0.0975303952680933,0.));
#13897=DIRECTION('',(0.,0.,-1.));
#13898=DIRECTION('center_axis',(1.23321574121574E-16,-1.,0.));
#13899=DIRECTION('ref_axis',(1.,1.23321574121574E-16,0.));
#13900=DIRECTION('axis',(0.,0.,1.));
#13901=DIRECTION('refdir',(1.,0.,0.));
#13902=DIRECTION('center_axis',(0.,0.,-1.));
#13903=DIRECTION('ref_axis',(-1.,0.,0.));
#13904=DIRECTION('center_axis',(0.,0.,1.));
#13905=DIRECTION('ref_axis',(1.,0.,0.));
#13906=DIRECTION('',(0.,0.,-1.));
#13907=DIRECTION('center_axis',(0.,0.,1.));
#13908=DIRECTION('ref_axis',(1.,0.,0.));
#13909=DIRECTION('',(0.,0.,-1.));
#13910=DIRECTION('center_axis',(0.,0.,1.));
#13911=DIRECTION('ref_axis',(1.,0.,0.));
#13912=DIRECTION('',(0.867884643612355,0.496765785236721,0.));
#13913=DIRECTION('',(0.867884643612355,-0.496765785236721,0.));
#13914=DIRECTION('',(1.,0.,0.));
#13915=DIRECTION('',(0.706716667923105,-0.707496679341793,0.));
#13916=DIRECTION('',(0.,-1.,0.));
#13917=DIRECTION('center_axis',(0.,0.,-1.));
#13918=DIRECTION('ref_axis',(1.,0.,0.));
#13919=DIRECTION('',(-1.,0.,0.));
#13920=DIRECTION('center_axis',(0.,0.,1.));
#13921=DIRECTION('ref_axis',(1.,0.,0.));
#13922=DIRECTION('',(1.54197609341422E-14,-1.,0.));
#13923=DIRECTION('center_axis',(0.,0.,1.));
#13924=DIRECTION('ref_axis',(1.,0.,0.));
#13925=DIRECTION('',(1.,0.,0.));
#13926=DIRECTION('center_axis',(0.,0.,-1.));
#13927=DIRECTION('ref_axis',(1.,0.,0.));
#13928=DIRECTION('',(0.,-1.,0.));
#13929=DIRECTION('center_axis',(0.,0.,1.));
#13930=DIRECTION('ref_axis',(1.,0.,0.));
#13931=DIRECTION('',(1.,1.68215601615235E-15,0.));
#13932=DIRECTION('center_axis',(0.,0.,1.));
#13933=DIRECTION('ref_axis',(1.,0.,0.));
#13934=DIRECTION('',(-1.68215592970338E-15,1.,0.));
#13935=DIRECTION('center_axis',(0.,0.,1.));
#13936=DIRECTION('ref_axis',(1.,0.,0.));
#13937=DIRECTION('',(-1.,1.38779120854827E-13,0.));
#13938=DIRECTION('center_axis',(0.,0.,-1.));
#13939=DIRECTION('ref_axis',(1.,0.,0.));
#13940=DIRECTION('',(0.,1.,0.));
#13941=DIRECTION('center_axis',(0.,0.,1.));
#13942=DIRECTION('ref_axis',(1.,0.,0.));
#13943=DIRECTION('',(-1.,-7.70988123297925E-15,0.));
#13944=DIRECTION('center_axis',(0.,0.,1.));
#13945=DIRECTION('ref_axis',(1.,0.,0.));
#13946=DIRECTION('',(0.,-1.,0.));
#13947=DIRECTION('center_axis',(0.,0.,-1.));
#13948=DIRECTION('ref_axis',(1.,0.,0.));
#13949=DIRECTION('',(-1.,2.72113516754055E-15,0.));
#13950=DIRECTION('',(-0.707106781186546,0.707106781186549,0.));
#13951=DIRECTION('',(0.,1.,0.));
#13952=DIRECTION('',(-0.499998732686741,0.866026135466853,0.));
#13953=DIRECTION('',(0.499998732686741,0.866026135466853,0.));
#13954=DIRECTION('',(0.,1.,0.));
#13955=DIRECTION('',(0.707106781186546,0.707106781186549,0.));
#13956=DIRECTION('',(1.,0.,0.));
#13957=DIRECTION('center_axis',(0.,0.,-1.));
#13958=DIRECTION('ref_axis',(1.,0.,0.));
#13959=DIRECTION('',(0.,-1.,0.));
#13960=DIRECTION('center_axis',(0.,0.,1.));
#13961=DIRECTION('ref_axis',(1.,0.,0.));
#13962=DIRECTION('',(1.,0.,0.));
#13963=DIRECTION('center_axis',(0.,0.,1.));
#13964=DIRECTION('ref_axis',(1.,0.,0.));
#13965=DIRECTION('',(0.,1.,0.));
#13966=DIRECTION('center_axis',(0.,0.,-1.));
#13967=DIRECTION('ref_axis',(1.,0.,0.));
#13968=DIRECTION('',(1.,6.93895604274136E-14,0.));
#13969=DIRECTION('center_axis',(0.,0.,1.));
#13970=DIRECTION('ref_axis',(1.,0.,0.));
#13971=DIRECTION('',(-1.68215592970338E-15,1.,0.));
#13972=DIRECTION('center_axis',(0.,0.,1.));
#13973=DIRECTION('ref_axis',(1.,0.,0.));
#13974=DIRECTION('',(-1.,0.,0.));
#13975=DIRECTION('center_axis',(0.,0.,1.));
#13976=DIRECTION('ref_axis',(1.,0.,0.));
#13977=DIRECTION('',(0.,-1.,0.));
#13978=DIRECTION('center_axis',(0.,0.,-1.));
#13979=DIRECTION('ref_axis',(1.,0.,0.));
#13980=DIRECTION('',(-1.,0.,0.));
#13981=DIRECTION('center_axis',(0.,0.,1.));
#13982=DIRECTION('ref_axis',(1.,0.,0.));
#13983=DIRECTION('',(0.,-1.,0.));
#13984=DIRECTION('center_axis',(0.,0.,1.));
#13985=DIRECTION('ref_axis',(1.,0.,0.));
#13986=DIRECTION('',(1.,-2.04085131219443E-15,0.));
#13987=DIRECTION('center_axis',(0.,0.,-1.));
#13988=DIRECTION('ref_axis',(1.,0.,0.));
#13989=DIRECTION('',(0.,-1.,0.));
#13990=DIRECTION('',(-0.706716667923105,-0.707496679341793,0.));
#13991=DIRECTION('',(-1.,0.,0.));
#13992=DIRECTION('',(-0.867884643612358,-0.496765785236715,0.));
#13993=DIRECTION('',(-0.867884643612358,0.496765785236715,0.));
#13994=DIRECTION('',(-1.,0.,0.));
#13995=DIRECTION('',(-0.706716667923105,0.707496679341793,0.));
#13996=DIRECTION('',(-5.4422705895004E-15,1.,0.));
#13997=DIRECTION('center_axis',(0.,0.,-1.));
#13998=DIRECTION('ref_axis',(1.,0.,0.));
#13999=DIRECTION('',(1.,0.,0.));
#14000=DIRECTION('center_axis',(0.,0.,1.));
#14001=DIRECTION('ref_axis',(1.,0.,0.));
#14002=DIRECTION('',(-1.54197609341422E-14,1.,0.));
#14003=DIRECTION('center_axis',(0.,0.,1.));
#14004=DIRECTION('ref_axis',(1.,0.,0.));
#14005=DIRECTION('',(-1.,0.,0.));
#14006=DIRECTION('center_axis',(0.,0.,-1.));
#14007=DIRECTION('ref_axis',(1.,0.,0.));
#14008=DIRECTION('',(0.,1.,0.));
#14009=DIRECTION('center_axis',(0.,0.,1.));
#14010=DIRECTION('ref_axis',(1.,0.,0.));
#14011=DIRECTION('',(-1.,-1.68215601615234E-15,0.));
#14012=DIRECTION('center_axis',(0.,0.,1.));
#14013=DIRECTION('ref_axis',(1.,0.,0.));
#14014=DIRECTION('',(1.68215592970338E-15,-1.,0.));
#14015=DIRECTION('center_axis',(0.,0.,1.));
#14016=DIRECTION('ref_axis',(1.,0.,0.));
#14017=DIRECTION('',(1.,-1.38779120854846E-13,0.));
#14018=DIRECTION('center_axis',(0.,0.,-1.));
#14019=DIRECTION('ref_axis',(1.,0.,0.));
#14020=DIRECTION('',(0.,-1.,0.));
#14021=DIRECTION('center_axis',(0.,0.,1.));
#14022=DIRECTION('ref_axis',(1.,0.,0.));
#14023=DIRECTION('',(1.,7.70988123297925E-15,0.));
#14024=DIRECTION('center_axis',(0.,0.,1.));
#14025=DIRECTION('ref_axis',(1.,0.,0.));
#14026=DIRECTION('',(-4.0817021727476E-15,1.,0.));
#14027=DIRECTION('center_axis',(0.,0.,-1.));
#14028=DIRECTION('ref_axis',(1.,0.,0.));
#14029=DIRECTION('',(1.,-2.72113516754055E-15,0.));
#14030=DIRECTION('',(0.707106781186547,-0.707106781186547,0.));
#14031=DIRECTION('',(0.,-1.,0.));
#14032=DIRECTION('',(0.499998732686731,-0.866026135466859,0.));
#14033=DIRECTION('',(-0.499998732686731,-0.866026135466859,0.));
#14034=DIRECTION('',(0.,-1.,0.));
#14035=DIRECTION('',(-0.707106781186547,-0.707106781186548,0.));
#14036=DIRECTION('',(-1.,0.,0.));
#14037=DIRECTION('center_axis',(0.,0.,-1.));
#14038=DIRECTION('ref_axis',(1.,0.,0.));
#14039=DIRECTION('',(0.,1.,0.));
#14040=DIRECTION('center_axis',(0.,0.,1.));
#14041=DIRECTION('ref_axis',(1.,0.,0.));
#14042=DIRECTION('',(-1.,-7.70988123297925E-15,0.));
#14043=DIRECTION('center_axis',(0.,0.,1.));
#14044=DIRECTION('ref_axis',(1.,0.,0.));
#14045=DIRECTION('',(0.,-1.,0.));
#14046=DIRECTION('center_axis',(0.,0.,-1.));
#14047=DIRECTION('ref_axis',(1.,0.,0.));
#14048=DIRECTION('',(-1.,-6.93895604274136E-14,0.));
#14049=DIRECTION('center_axis',(0.,0.,1.));
#14050=DIRECTION('ref_axis',(1.,0.,0.));
#14051=DIRECTION('',(1.68215592970338E-15,-1.,0.));
#14052=DIRECTION('center_axis',(0.,0.,1.));
#14053=DIRECTION('ref_axis',(1.,0.,0.));
#14054=DIRECTION('',(1.,0.,0.));
#14055=DIRECTION('center_axis',(0.,0.,1.));
#14056=DIRECTION('ref_axis',(1.,0.,0.));
#14057=DIRECTION('',(0.,1.,0.));
#14058=DIRECTION('center_axis',(0.,0.,-1.));
#14059=DIRECTION('ref_axis',(1.,0.,0.));
#14060=DIRECTION('',(1.,-3.46945490866966E-14,0.));
#14061=DIRECTION('center_axis',(0.,0.,1.));
#14062=DIRECTION('ref_axis',(1.,0.,0.));
#14063=DIRECTION('',(-1.54197609341422E-14,1.,0.));
#14064=DIRECTION('center_axis',(0.,0.,1.));
#14065=DIRECTION('ref_axis',(1.,0.,0.));
#14066=DIRECTION('',(-1.,1.0204256560972E-15,0.));
#14067=DIRECTION('center_axis',(0.,0.,-1.));
#14068=DIRECTION('ref_axis',(1.,0.,0.));
#14069=DIRECTION('',(0.,1.,0.));
#14070=DIRECTION('',(0.706716667923104,0.707496679341793,0.));
#14071=DIRECTION('',(1.,-2.09985316358847E-15,0.));
#14072=DIRECTION('',(-1.,0.,0.));
#14073=DIRECTION('center_axis',(0.,0.,1.));
#14074=DIRECTION('ref_axis',(1.,0.,0.));
#14075=DIRECTION('',(-6.30808317960405E-15,1.,0.));
#14076=DIRECTION('center_axis',(0.,0.,1.));
#14077=DIRECTION('ref_axis',(1.,0.,0.));
#14078=DIRECTION('',(1.,3.15404158980207E-15,0.));
#14079=DIRECTION('center_axis',(0.,0.,1.));
#14080=DIRECTION('ref_axis',(1.,0.,0.));
#14081=DIRECTION('',(0.,-1.,0.));
#14082=DIRECTION('center_axis',(0.,0.,1.));
#14083=DIRECTION('ref_axis',(1.,0.,0.));
#14084=DIRECTION('',(-0.778588686672397,0.627534586286487,0.));
#14085=DIRECTION('center_axis',(0.,0.,1.));
#14086=DIRECTION('ref_axis',(1.,0.,0.));
#14087=DIRECTION('',(-0.778588686672393,-0.627534586286492,0.));
#14088=DIRECTION('center_axis',(0.,0.,1.));
#14089=DIRECTION('ref_axis',(1.,0.,0.));
#14090=DIRECTION('',(0.61886791399197,0.785495070023503,0.));
#14091=DIRECTION('center_axis',(0.,0.,1.));
#14092=DIRECTION('ref_axis',(1.,0.,0.));
#14093=DIRECTION('',(-0.618867913991998,0.785495070023481,0.));
#14094=DIRECTION('center_axis',(0.,0.,1.));
#14095=DIRECTION('ref_axis',(1.,0.,0.));
#14096=DIRECTION('',(0.778588686672382,-0.627534586286505,0.));
#14097=DIRECTION('center_axis',(0.,0.,1.));
#14098=DIRECTION('ref_axis',(1.,0.,0.));
#14099=DIRECTION('',(0.778588686672372,0.627534586286517,0.));
#14100=DIRECTION('center_axis',(0.,0.,1.));
#14101=DIRECTION('ref_axis',(1.,0.,0.));
#14102=DIRECTION('',(-0.61886791399199,-0.785495070023487,0.));
#14103=DIRECTION('',(0.61886791399197,-0.785495070023503,0.));
#14104=DIRECTION('center_axis',(0.,0.,1.));
#14105=DIRECTION('ref_axis',(1.,0.,0.));
#14106=DIRECTION('',(1.,0.,0.));
#14107=DIRECTION('center_axis',(0.,0.,1.));
#14108=DIRECTION('ref_axis',(1.,0.,0.));
#14109=DIRECTION('',(6.30808317960409E-15,-1.,0.));
#14110=DIRECTION('center_axis',(0.,0.,1.));
#14111=DIRECTION('ref_axis',(1.,0.,0.));
#14112=DIRECTION('',(-1.,-3.15404158980205E-15,0.));
#14113=DIRECTION('center_axis',(0.,0.,1.));
#14114=DIRECTION('ref_axis',(1.,0.,0.));
#14115=DIRECTION('',(0.,1.,0.));
#14116=DIRECTION('center_axis',(0.,0.,1.));
#14117=DIRECTION('ref_axis',(1.,0.,0.));
#14118=DIRECTION('',(-6.30808317960404E-15,1.,0.));
#14119=DIRECTION('center_axis',(0.,0.,1.));
#14120=DIRECTION('ref_axis',(1.,0.,0.));
#14121=DIRECTION('',(1.,3.15404158980205E-15,0.));
#14122=DIRECTION('center_axis',(0.,0.,1.));
#14123=DIRECTION('ref_axis',(1.,0.,0.));
#14124=DIRECTION('',(0.,-1.,0.));
#14125=DIRECTION('center_axis',(0.,0.,1.));
#14126=DIRECTION('ref_axis',(1.,0.,0.));
#14127=DIRECTION('',(-1.,0.,0.));
#14128=DIRECTION('center_axis',(0.,0.,1.));
#14129=DIRECTION('ref_axis',(1.,0.,0.));
#14130=DIRECTION('',(-1.,0.,0.));
#14131=DIRECTION('center_axis',(0.,0.,1.));
#14132=DIRECTION('ref_axis',(1.,0.,0.));
#14133=DIRECTION('',(0.,1.,0.));
#14134=DIRECTION('center_axis',(0.,0.,1.));
#14135=DIRECTION('ref_axis',(1.,0.,0.));
#14136=DIRECTION('',(1.,0.,0.));
#14137=DIRECTION('center_axis',(0.,0.,1.));
#14138=DIRECTION('ref_axis',(1.,0.,0.));
#14139=DIRECTION('',(6.30808317960409E-15,-1.,0.));
#14140=DIRECTION('center_axis',(0.,0.,1.));
#14141=DIRECTION('ref_axis',(1.,0.,0.));
#14142=DIRECTION('center_axis',(0.,0.,1.));
#14143=DIRECTION('ref_axis',(1.,0.,0.));
#14144=DIRECTION('',(0.867884643612355,0.496765785236721,0.));
#14145=DIRECTION('',(1.,-2.09985316358847E-15,0.));
#14146=DIRECTION('',(0.706716667923104,0.707496679341793,0.));
#14147=DIRECTION('',(0.,1.,0.));
#14148=DIRECTION('center_axis',(0.,0.,-1.));
#14149=DIRECTION('ref_axis',(1.,0.,0.));
#14150=DIRECTION('',(-1.,1.0204256560972E-15,0.));
#14151=DIRECTION('center_axis',(0.,0.,1.));
#14152=DIRECTION('ref_axis',(1.,0.,0.));
#14153=DIRECTION('',(-1.54197609341422E-14,1.,0.));
#14154=DIRECTION('center_axis',(0.,0.,1.));
#14155=DIRECTION('ref_axis',(1.,0.,0.));
#14156=DIRECTION('',(1.,-3.46945490866966E-14,0.));
#14157=DIRECTION('center_axis',(0.,0.,-1.));
#14158=DIRECTION('ref_axis',(1.,0.,0.));
#14159=DIRECTION('',(0.,1.,0.));
#14160=DIRECTION('center_axis',(0.,0.,1.));
#14161=DIRECTION('ref_axis',(1.,0.,0.));
#14162=DIRECTION('',(1.,0.,0.));
#14163=DIRECTION('center_axis',(0.,0.,1.));
#14164=DIRECTION('ref_axis',(1.,0.,0.));
#14165=DIRECTION('',(1.68215592970338E-15,-1.,0.));
#14166=DIRECTION('center_axis',(0.,0.,1.));
#14167=DIRECTION('ref_axis',(1.,0.,0.));
#14168=DIRECTION('',(-1.,-6.93895604274136E-14,0.));
#14169=DIRECTION('center_axis',(0.,0.,-1.));
#14170=DIRECTION('ref_axis',(1.,0.,0.));
#14171=DIRECTION('',(0.,-1.,0.));
#14172=DIRECTION('center_axis',(0.,0.,1.));
#14173=DIRECTION('ref_axis',(1.,0.,0.));
#14174=DIRECTION('',(-1.,-7.70988123297925E-15,0.));
#14175=DIRECTION('center_axis',(0.,0.,1.));
#14176=DIRECTION('ref_axis',(1.,0.,0.));
#14177=DIRECTION('',(0.,1.,0.));
#14178=DIRECTION('center_axis',(0.,0.,-1.));
#14179=DIRECTION('ref_axis',(1.,0.,0.));
#14180=DIRECTION('',(-1.,0.,0.));
#14181=DIRECTION('',(-0.707106781186547,-0.707106781186548,0.));
#14182=DIRECTION('',(0.,-1.,0.));
#14183=DIRECTION('',(-0.499998732686731,-0.866026135466859,0.));
#14184=DIRECTION('',(0.499998732686731,-0.866026135466859,0.));
#14185=DIRECTION('',(0.,-1.,0.));
#14186=DIRECTION('',(0.707106781186547,-0.707106781186547,0.));
#14187=DIRECTION('',(1.,-2.72113516754055E-15,0.));
#14188=DIRECTION('center_axis',(0.,0.,-1.));
#14189=DIRECTION('ref_axis',(1.,0.,0.));
#14190=DIRECTION('',(-4.0817021727476E-15,1.,0.));
#14191=DIRECTION('center_axis',(0.,0.,1.));
#14192=DIRECTION('ref_axis',(1.,0.,0.));
#14193=DIRECTION('',(1.,7.70988123297925E-15,0.));
#14194=DIRECTION('center_axis',(0.,0.,1.));
#14195=DIRECTION('ref_axis',(1.,0.,0.));
#14196=DIRECTION('',(0.,-1.,0.));
#14197=DIRECTION('center_axis',(0.,0.,-1.));
#14198=DIRECTION('ref_axis',(1.,0.,0.));
#14199=DIRECTION('',(1.,-1.38779120854846E-13,0.));
#14200=DIRECTION('center_axis',(0.,0.,1.));
#14201=DIRECTION('ref_axis',(1.,0.,0.));
#14202=DIRECTION('',(1.68215592970338E-15,-1.,0.));
#14203=DIRECTION('center_axis',(0.,0.,1.));
#14204=DIRECTION('ref_axis',(1.,0.,0.));
#14205=DIRECTION('',(-1.,-1.68215601615234E-15,0.));
#14206=DIRECTION('center_axis',(0.,0.,1.));
#14207=DIRECTION('ref_axis',(1.,0.,0.));
#14208=DIRECTION('',(0.,1.,0.));
#14209=DIRECTION('center_axis',(0.,0.,-1.));
#14210=DIRECTION('ref_axis',(1.,0.,0.));
#14211=DIRECTION('',(-1.,0.,0.));
#14212=DIRECTION('center_axis',(0.,0.,1.));
#14213=DIRECTION('ref_axis',(1.,0.,0.));
#14214=DIRECTION('',(-1.54197609341422E-14,1.,0.));
#14215=DIRECTION('center_axis',(0.,0.,1.));
#14216=DIRECTION('ref_axis',(1.,0.,0.));
#14217=DIRECTION('',(1.,0.,0.));
#14218=DIRECTION('center_axis',(0.,0.,-1.));
#14219=DIRECTION('ref_axis',(1.,0.,0.));
#14220=DIRECTION('',(-5.4422705895004E-15,1.,0.));
#14221=DIRECTION('',(-0.706716667923105,0.707496679341793,0.));
#14222=DIRECTION('',(-1.,0.,0.));
#14223=DIRECTION('',(-0.867884643612358,0.496765785236715,0.));
#14224=DIRECTION('',(-0.867884643612358,-0.496765785236715,0.));
#14225=DIRECTION('',(-1.,0.,0.));
#14226=DIRECTION('',(-0.706716667923105,-0.707496679341793,0.));
#14227=DIRECTION('',(0.,-1.,0.));
#14228=DIRECTION('center_axis',(0.,0.,-1.));
#14229=DIRECTION('ref_axis',(1.,0.,0.));
#14230=DIRECTION('',(1.,-2.04085131219443E-15,0.));
#14231=DIRECTION('center_axis',(0.,0.,1.));
#14232=DIRECTION('ref_axis',(1.,0.,0.));
#14233=DIRECTION('',(0.,-1.,0.));
#14234=DIRECTION('center_axis',(0.,0.,1.));
#14235=DIRECTION('ref_axis',(1.,0.,0.));
#14236=DIRECTION('',(-1.,0.,0.));
#14237=DIRECTION('center_axis',(0.,0.,-1.));
#14238=DIRECTION('ref_axis',(1.,0.,0.));
#14239=DIRECTION('',(0.,-1.,0.));
#14240=DIRECTION('center_axis',(0.,0.,1.));
#14241=DIRECTION('ref_axis',(1.,0.,0.));
#14242=DIRECTION('',(-1.,0.,0.));
#14243=DIRECTION('center_axis',(0.,0.,1.));
#14244=DIRECTION('ref_axis',(1.,0.,0.));
#14245=DIRECTION('',(-1.68215592970338E-15,1.,0.));
#14246=DIRECTION('center_axis',(0.,0.,1.));
#14247=DIRECTION('ref_axis',(1.,0.,0.));
#14248=DIRECTION('',(1.,6.93895604274136E-14,0.));
#14249=DIRECTION('center_axis',(0.,0.,-1.));
#14250=DIRECTION('ref_axis',(1.,0.,0.));
#14251=DIRECTION('',(0.,1.,0.));
#14252=DIRECTION('center_axis',(0.,0.,1.));
#14253=DIRECTION('ref_axis',(1.,0.,0.));
#14254=DIRECTION('',(1.,0.,0.));
#14255=DIRECTION('center_axis',(0.,0.,1.));
#14256=DIRECTION('ref_axis',(1.,0.,0.));
#14257=DIRECTION('',(0.,-1.,0.));
#14258=DIRECTION('center_axis',(0.,0.,-1.));
#14259=DIRECTION('ref_axis',(1.,0.,0.));
#14260=DIRECTION('',(1.,0.,0.));
#14261=DIRECTION('',(0.707106781186546,0.707106781186549,0.));
#14262=DIRECTION('',(0.,1.,0.));
#14263=DIRECTION('',(0.499998732686741,0.866026135466853,0.));
#14264=DIRECTION('',(-0.499998732686741,0.866026135466853,0.));
#14265=DIRECTION('',(0.,1.,0.));
#14266=DIRECTION('',(-0.707106781186546,0.707106781186549,0.));
#14267=DIRECTION('',(-1.,2.72113516754055E-15,0.));
#14268=DIRECTION('center_axis',(0.,0.,-1.));
#14269=DIRECTION('ref_axis',(1.,0.,0.));
#14270=DIRECTION('',(0.,-1.,0.));
#14271=DIRECTION('center_axis',(0.,0.,1.));
#14272=DIRECTION('ref_axis',(1.,0.,0.));
#14273=DIRECTION('',(-1.,-7.70988123297925E-15,0.));
#14274=DIRECTION('center_axis',(0.,0.,1.));
#14275=DIRECTION('ref_axis',(1.,0.,0.));
#14276=DIRECTION('',(0.,1.,0.));
#14277=DIRECTION('center_axis',(0.,0.,-1.));
#14278=DIRECTION('ref_axis',(1.,0.,0.));
#14279=DIRECTION('',(-1.,1.38779120854827E-13,0.));
#14280=DIRECTION('center_axis',(0.,0.,1.));
#14281=DIRECTION('ref_axis',(1.,0.,0.));
#14282=DIRECTION('',(-1.68215592970338E-15,1.,0.));
#14283=DIRECTION('center_axis',(0.,0.,1.));
#14284=DIRECTION('ref_axis',(1.,0.,0.));
#14285=DIRECTION('',(1.,1.68215601615235E-15,0.));
#14286=DIRECTION('center_axis',(0.,0.,1.));
#14287=DIRECTION('ref_axis',(1.,0.,0.));
#14288=DIRECTION('',(0.,-1.,0.));
#14289=DIRECTION('center_axis',(0.,0.,-1.));
#14290=DIRECTION('ref_axis',(1.,0.,0.));
#14291=DIRECTION('',(1.,0.,0.));
#14292=DIRECTION('center_axis',(0.,0.,1.));
#14293=DIRECTION('ref_axis',(1.,0.,0.));
#14294=DIRECTION('',(1.54197609341422E-14,-1.,0.));
#14295=DIRECTION('center_axis',(0.,0.,1.));
#14296=DIRECTION('ref_axis',(1.,0.,0.));
#14297=DIRECTION('',(-1.,0.,0.));
#14298=DIRECTION('center_axis',(0.,0.,-1.));
#14299=DIRECTION('ref_axis',(1.,0.,0.));
#14300=DIRECTION('',(0.,-1.,0.));
#14301=DIRECTION('',(0.706716667923105,-0.707496679341793,0.));
#14302=DIRECTION('',(1.,0.,0.));
#14303=DIRECTION('',(0.867884643612355,-0.496765785236721,0.));
#14304=DIRECTION('center_axis',(0.,0.,1.));
#14305=DIRECTION('ref_axis',(1.,0.,0.));
#14306=DIRECTION('',(-1.,0.,0.));
#14307=DIRECTION('center_axis',(0.,0.,1.));
#14308=DIRECTION('ref_axis',(1.,0.,0.));
#14309=DIRECTION('',(0.,-1.,0.));
#14310=DIRECTION('center_axis',(0.,0.,1.));
#14311=DIRECTION('ref_axis',(1.,0.,0.));
#14312=DIRECTION('',(1.,3.15404158980207E-15,0.));
#14313=DIRECTION('center_axis',(0.,0.,1.));
#14314=DIRECTION('ref_axis',(1.,0.,0.));
#14315=DIRECTION('',(-6.30808317960405E-15,1.,0.));
#14316=DIRECTION('center_axis',(0.,0.,1.));
#14317=DIRECTION('ref_axis',(1.,0.,0.));
#14318=DIRECTION('',(1.,0.,0.));
#14319=DIRECTION('center_axis',(0.,0.,1.));
#14320=DIRECTION('ref_axis',(1.,0.,0.));
#14321=DIRECTION('',(0.,1.,0.));
#14322=DIRECTION('center_axis',(0.,0.,1.));
#14323=DIRECTION('ref_axis',(1.,0.,0.));
#14324=DIRECTION('',(-1.,-3.15404158980205E-15,0.));
#14325=DIRECTION('center_axis',(0.,0.,1.));
#14326=DIRECTION('ref_axis',(1.,0.,0.));
#14327=DIRECTION('',(6.30808317960409E-15,-1.,0.));
#14328=DIRECTION('center_axis',(0.,0.,1.));
#14329=DIRECTION('ref_axis',(1.,0.,0.));
#14330=DIRECTION('',(-1.,0.,0.));
#14331=DIRECTION('center_axis',(0.,0.,1.));
#14332=DIRECTION('ref_axis',(1.,0.,0.));
#14333=DIRECTION('',(6.30808317960409E-15,-1.,0.));
#14334=DIRECTION('center_axis',(0.,0.,1.));
#14335=DIRECTION('ref_axis',(1.,0.,0.));
#14336=DIRECTION('',(1.,0.,0.));
#14337=DIRECTION('center_axis',(0.,0.,1.));
#14338=DIRECTION('ref_axis',(1.,0.,0.));
#14339=DIRECTION('',(0.,1.,0.));
#14340=DIRECTION('center_axis',(0.,0.,1.));
#14341=DIRECTION('ref_axis',(1.,0.,0.));
#14342=DIRECTION('',(-6.30808317960404E-15,1.,0.));
#14343=DIRECTION('center_axis',(0.,0.,1.));
#14344=DIRECTION('ref_axis',(1.,0.,0.));
#14345=DIRECTION('',(-1.,0.,0.));
#14346=DIRECTION('center_axis',(0.,0.,1.));
#14347=DIRECTION('ref_axis',(1.,0.,0.));
#14348=DIRECTION('',(0.,-1.,0.));
#14349=DIRECTION('center_axis',(0.,0.,1.));
#14350=DIRECTION('ref_axis',(1.,0.,0.));
#14351=DIRECTION('',(1.,3.15404158980205E-15,0.));
#14352=DIRECTION('center_axis',(0.,0.,1.));
#14353=DIRECTION('ref_axis',(1.,0.,0.));
#14354=DIRECTION('',(-0.778588686672397,0.627534586286487,0.));
#14355=DIRECTION('center_axis',(0.,0.,1.));
#14356=DIRECTION('ref_axis',(1.,0.,0.));
#14357=DIRECTION('',(0.61886791399197,-0.785495070023503,0.));
#14358=DIRECTION('',(-0.61886791399199,-0.785495070023487,0.));
#14359=DIRECTION('center_axis',(0.,0.,1.));
#14360=DIRECTION('ref_axis',(1.,0.,0.));
#14361=DIRECTION('',(0.778588686672372,0.627534586286517,0.));
#14362=DIRECTION('center_axis',(0.,0.,1.));
#14363=DIRECTION('ref_axis',(1.,0.,0.));
#14364=DIRECTION('',(0.778588686672382,-0.627534586286505,0.));
#14365=DIRECTION('center_axis',(0.,0.,1.));
#14366=DIRECTION('ref_axis',(1.,0.,0.));
#14367=DIRECTION('',(-0.618867913991998,0.785495070023481,0.));
#14368=DIRECTION('center_axis',(0.,0.,1.));
#14369=DIRECTION('ref_axis',(1.,0.,0.));
#14370=DIRECTION('',(0.61886791399197,0.785495070023503,0.));
#14371=DIRECTION('center_axis',(0.,0.,1.));
#14372=DIRECTION('ref_axis',(1.,0.,0.));
#14373=DIRECTION('',(-0.778588686672393,-0.627534586286492,0.));
#14374=DIRECTION('center_axis',(-0.496765785236721,0.867884643612355,0.));
#14375=DIRECTION('ref_axis',(-0.867884643612355,-0.496765785236721,0.));
#14376=DIRECTION('',(0.,0.,-1.));
#14377=DIRECTION('',(0.,0.,-1.));
#14378=DIRECTION('center_axis',(0.496765785236721,0.867884643612355,0.));
#14379=DIRECTION('ref_axis',(-0.867884643612355,0.496765785236721,0.));
#14380=DIRECTION('',(0.,0.,-1.));
#14381=DIRECTION('center_axis',(0.,1.,0.));
#14382=DIRECTION('ref_axis',(0.,0.,1.));
#14383=DIRECTION('',(0.,0.,-1.));
#14384=DIRECTION('center_axis',(0.707496679341793,0.706716667923105,0.));
#14385=DIRECTION('ref_axis',(-0.706716667923105,0.707496679341793,0.));
#14386=DIRECTION('',(0.,0.,-1.));
#14387=DIRECTION('center_axis',(1.,0.,0.));
#14388=DIRECTION('ref_axis',(0.,0.,-1.));
#14389=DIRECTION('',(0.,0.,-1.));
#14390=DIRECTION('center_axis',(0.,0.,-1.));
#14391=DIRECTION('ref_axis',(-1.,0.,0.));
#14392=DIRECTION('',(0.,0.,-1.));
#14393=DIRECTION('center_axis',(0.,-1.,0.));
#14394=DIRECTION('ref_axis',(0.,0.,-1.));
#14395=DIRECTION('',(0.,0.,-1.));
#14396=DIRECTION('center_axis',(0.,0.,-1.));
#14397=DIRECTION('ref_axis',(-1.,0.,0.));
#14398=DIRECTION('',(0.,0.,-1.));
#14399=DIRECTION('center_axis',(1.,1.54197609341421E-14,0.));
#14400=DIRECTION('ref_axis',(-1.54197609341421E-14,1.,0.));
#14401=DIRECTION('',(0.,0.,-1.));
#14402=DIRECTION('center_axis',(0.,0.,-1.));
#14403=DIRECTION('ref_axis',(-1.,0.,0.));
#14404=DIRECTION('',(0.,0.,-1.));
#14405=DIRECTION('center_axis',(0.,1.,0.));
#14406=DIRECTION('ref_axis',(0.,0.,1.));
#14407=DIRECTION('',(0.,0.,-1.));
#14408=DIRECTION('center_axis',(0.,0.,-1.));
#14409=DIRECTION('ref_axis',(-1.,0.,0.));
#14410=DIRECTION('',(0.,0.,-1.));
#14411=DIRECTION('center_axis',(1.,0.,0.));
#14412=DIRECTION('ref_axis',(0.,0.,-1.));
#14413=DIRECTION('',(0.,0.,-1.));
#14414=DIRECTION('center_axis',(0.,0.,-1.));
#14415=DIRECTION('ref_axis',(-1.,0.,0.));
#14416=DIRECTION('',(0.,0.,-1.));
#14417=DIRECTION('center_axis',(-1.68215601615235E-15,1.,0.));
#14418=DIRECTION('ref_axis',(-1.,-1.68215601615235E-15,0.));
#14419=DIRECTION('',(0.,0.,-1.));
#14420=DIRECTION('center_axis',(0.,0.,-1.));
#14421=DIRECTION('ref_axis',(-1.,0.,0.));
#14422=DIRECTION('',(0.,0.,-1.));
#14423=DIRECTION('center_axis',(-1.,-1.68215592970338E-15,0.));
#14424=DIRECTION('ref_axis',(1.68215592970338E-15,-1.,0.));
#14425=DIRECTION('',(0.,0.,-1.));
#14426=DIRECTION('center_axis',(0.,0.,-1.));
#14427=DIRECTION('ref_axis',(-1.,0.,0.));
#14428=DIRECTION('',(0.,0.,-1.));
#14429=DIRECTION('center_axis',(-1.38779120854827E-13,-1.,0.));
#14430=DIRECTION('ref_axis',(1.,-1.38779120854827E-13,0.));
#14431=DIRECTION('',(0.,0.,-1.));
#14432=DIRECTION('center_axis',(0.,0.,-1.));
#14433=DIRECTION('ref_axis',(-1.,0.,0.));
#14434=DIRECTION('',(0.,0.,-1.));
#14435=DIRECTION('center_axis',(-1.,0.,0.));
#14436=DIRECTION('ref_axis',(0.,0.,1.));
#14437=DIRECTION('',(0.,0.,-1.));
#14438=DIRECTION('center_axis',(0.,0.,-1.));
#14439=DIRECTION('ref_axis',(-1.,0.,0.));
#14440=DIRECTION('',(0.,0.,-1.));
#14441=DIRECTION('center_axis',(7.70988123297925E-15,-1.,0.));
#14442=DIRECTION('ref_axis',(1.,7.70988123297925E-15,0.));
#14443=DIRECTION('',(0.,0.,-1.));
#14444=DIRECTION('center_axis',(0.,0.,-1.));
#14445=DIRECTION('ref_axis',(-1.,0.,0.));
#14446=DIRECTION('',(0.,0.,-1.));
#14447=DIRECTION('center_axis',(1.,0.,0.));
#14448=DIRECTION('ref_axis',(0.,0.,-1.));
#14449=DIRECTION('',(0.,0.,-1.));
#14450=DIRECTION('center_axis',(0.,0.,-1.));
#14451=DIRECTION('ref_axis',(-1.,0.,0.));
#14452=DIRECTION('',(0.,0.,-1.));
#14453=DIRECTION('center_axis',(-2.72113516754055E-15,-1.,0.));
#14454=DIRECTION('ref_axis',(1.,-2.72113516754055E-15,0.));
#14455=DIRECTION('',(0.,0.,-1.));
#14456=DIRECTION('center_axis',(-0.707106781186549,-0.707106781186546,0.));
#14457=DIRECTION('ref_axis',(0.707106781186546,-0.707106781186549,0.));
#14458=DIRECTION('',(0.,0.,-1.));
#14459=DIRECTION('center_axis',(-1.,0.,0.));
#14460=DIRECTION('ref_axis',(0.,0.,1.));
#14461=DIRECTION('',(0.,0.,-1.));
#14462=DIRECTION('center_axis',(-0.866026135466853,-0.499998732686741,0.));
#14463=DIRECTION('ref_axis',(0.499998732686741,-0.866026135466854,0.));
#14464=DIRECTION('',(0.,0.,-1.));
#14465=DIRECTION('center_axis',(-0.866026135466853,0.499998732686741,0.));
#14466=DIRECTION('ref_axis',(-0.499998732686741,-0.866026135466854,0.));
#14467=DIRECTION('',(0.,0.,-1.));
#14468=DIRECTION('center_axis',(-1.,0.,0.));
#14469=DIRECTION('ref_axis',(0.,0.,1.));
#14470=DIRECTION('',(0.,0.,-1.));
#14471=DIRECTION('center_axis',(-0.707106781186549,0.707106781186546,0.));
#14472=DIRECTION('ref_axis',(-0.707106781186546,-0.707106781186549,0.));
#14473=DIRECTION('',(0.,0.,-1.));
#14474=DIRECTION('center_axis',(0.,1.,0.));
#14475=DIRECTION('ref_axis',(0.,0.,1.));
#14476=DIRECTION('',(0.,0.,-1.));
#14477=DIRECTION('center_axis',(0.,0.,-1.));
#14478=DIRECTION('ref_axis',(-1.,0.,0.));
#14479=DIRECTION('',(0.,0.,-1.));
#14480=DIRECTION('center_axis',(1.,0.,0.));
#14481=DIRECTION('ref_axis',(0.,0.,-1.));
#14482=DIRECTION('',(0.,0.,-1.));
#14483=DIRECTION('center_axis',(0.,0.,-1.));
#14484=DIRECTION('ref_axis',(-1.,0.,0.));
#14485=DIRECTION('',(0.,0.,-1.));
#14486=DIRECTION('center_axis',(0.,1.,0.));
#14487=DIRECTION('ref_axis',(0.,0.,1.));
#14488=DIRECTION('',(0.,0.,-1.));
#14489=DIRECTION('center_axis',(0.,0.,-1.));
#14490=DIRECTION('ref_axis',(-1.,0.,0.));
#14491=DIRECTION('',(0.,0.,-1.));
#14492=DIRECTION('center_axis',(-1.,0.,0.));
#14493=DIRECTION('ref_axis',(0.,0.,1.));
#14494=DIRECTION('',(0.,0.,-1.));
#14495=DIRECTION('center_axis',(0.,0.,-1.));
#14496=DIRECTION('ref_axis',(-1.,0.,0.));
#14497=DIRECTION('',(0.,0.,-1.));
#14498=DIRECTION('center_axis',(-6.93895604274136E-14,1.,0.));
#14499=DIRECTION('ref_axis',(-1.,-6.93895604274136E-14,0.));
#14500=DIRECTION('',(0.,0.,-1.));
#14501=DIRECTION('center_axis',(0.,0.,-1.));
#14502=DIRECTION('ref_axis',(-1.,0.,0.));
#14503=DIRECTION('',(0.,0.,-1.));
#14504=DIRECTION('center_axis',(-1.,-1.68215592970338E-15,0.));
#14505=DIRECTION('ref_axis',(1.68215592970338E-15,-1.,0.));
#14506=DIRECTION('',(0.,0.,-1.));
#14507=DIRECTION('center_axis',(0.,0.,-1.));
#14508=DIRECTION('ref_axis',(-1.,0.,0.));
#14509=DIRECTION('',(0.,0.,-1.));
#14510=DIRECTION('center_axis',(0.,-1.,0.));
#14511=DIRECTION('ref_axis',(0.,0.,-1.));
#14512=DIRECTION('',(0.,0.,-1.));
#14513=DIRECTION('center_axis',(0.,0.,-1.));
#14514=DIRECTION('ref_axis',(-1.,0.,0.));
#14515=DIRECTION('',(0.,0.,-1.));
#14516=DIRECTION('center_axis',(1.,0.,0.));
#14517=DIRECTION('ref_axis',(0.,0.,-1.));
#14518=DIRECTION('',(0.,0.,-1.));
#14519=DIRECTION('center_axis',(0.,0.,-1.));
#14520=DIRECTION('ref_axis',(-1.,0.,0.));
#14521=DIRECTION('',(0.,0.,-1.));
#14522=DIRECTION('center_axis',(0.,-1.,0.));
#14523=DIRECTION('ref_axis',(0.,0.,-1.));
#14524=DIRECTION('',(0.,0.,-1.));
#14525=DIRECTION('center_axis',(0.,0.,-1.));
#14526=DIRECTION('ref_axis',(-1.,0.,0.));
#14527=DIRECTION('',(0.,0.,-1.));
#14528=DIRECTION('center_axis',(1.,0.,0.));
#14529=DIRECTION('ref_axis',(0.,0.,-1.));
#14530=DIRECTION('',(0.,0.,-1.));
#14531=DIRECTION('center_axis',(0.,0.,-1.));
#14532=DIRECTION('ref_axis',(-1.,0.,0.));
#14533=DIRECTION('',(0.,0.,-1.));
#14534=DIRECTION('center_axis',(2.04085131219443E-15,1.,0.));
#14535=DIRECTION('ref_axis',(-1.,2.04085131219443E-15,0.));
#14536=DIRECTION('',(0.,0.,-1.));
#14537=DIRECTION('center_axis',(0.,0.,-1.));
#14538=DIRECTION('ref_axis',(-1.,0.,0.));
#14539=DIRECTION('',(0.,0.,-1.));
#14540=DIRECTION('center_axis',(1.,0.,0.));
#14541=DIRECTION('ref_axis',(0.,0.,-1.));
#14542=DIRECTION('',(0.,0.,-1.));
#14543=DIRECTION('center_axis',(0.707496679341793,-0.706716667923105,0.));
#14544=DIRECTION('ref_axis',(0.706716667923105,0.707496679341793,0.));
#14545=DIRECTION('',(0.,0.,-1.));
#14546=DIRECTION('center_axis',(0.,-1.,0.));
#14547=DIRECTION('ref_axis',(0.,0.,-1.));
#14548=DIRECTION('',(0.,0.,-1.));
#14549=DIRECTION('center_axis',(0.496765785236716,-0.867884643612358,0.));
#14550=DIRECTION('ref_axis',(0.867884643612358,0.496765785236716,0.));
#14551=DIRECTION('',(0.,0.,-1.));
#14552=DIRECTION('center_axis',(-0.496765785236716,-0.867884643612358,0.));
#14553=DIRECTION('ref_axis',(0.867884643612358,-0.496765785236716,0.));
#14554=DIRECTION('',(0.,0.,-1.));
#14555=DIRECTION('center_axis',(0.,-1.,0.));
#14556=DIRECTION('ref_axis',(0.,0.,-1.));
#14557=DIRECTION('',(0.,0.,-1.));
#14558=DIRECTION('center_axis',(-0.707496679341793,-0.706716667923105,0.));
#14559=DIRECTION('ref_axis',(0.706716667923105,-0.707496679341793,0.));
#14560=DIRECTION('',(0.,0.,-1.));
#14561=DIRECTION('center_axis',(-1.,-5.4422705895004E-15,0.));
#14562=DIRECTION('ref_axis',(5.4422705895004E-15,-1.,0.));
#14563=DIRECTION('',(0.,0.,-1.));
#14564=DIRECTION('center_axis',(0.,0.,-1.));
#14565=DIRECTION('ref_axis',(-1.,0.,0.));
#14566=DIRECTION('',(0.,0.,-1.));
#14567=DIRECTION('center_axis',(0.,1.,0.));
#14568=DIRECTION('ref_axis',(0.,0.,1.));
#14569=DIRECTION('',(0.,0.,-1.));
#14570=DIRECTION('center_axis',(0.,0.,-1.));
#14571=DIRECTION('ref_axis',(-1.,0.,0.));
#14572=DIRECTION('',(0.,0.,-1.));
#14573=DIRECTION('center_axis',(-1.,-1.54197609341422E-14,0.));
#14574=DIRECTION('ref_axis',(1.54197609341422E-14,-1.,0.));
#14575=DIRECTION('',(0.,0.,-1.));
#14576=DIRECTION('center_axis',(0.,0.,-1.));
#14577=DIRECTION('ref_axis',(-1.,0.,0.));
#14578=DIRECTION('',(0.,0.,-1.));
#14579=DIRECTION('center_axis',(0.,-1.,0.));
#14580=DIRECTION('ref_axis',(0.,0.,-1.));
#14581=DIRECTION('',(0.,0.,-1.));
#14582=DIRECTION('center_axis',(0.,0.,-1.));
#14583=DIRECTION('ref_axis',(-1.,0.,0.));
#14584=DIRECTION('',(0.,0.,-1.));
#14585=DIRECTION('center_axis',(-1.,0.,0.));
#14586=DIRECTION('ref_axis',(0.,0.,1.));
#14587=DIRECTION('',(0.,0.,-1.));
#14588=DIRECTION('center_axis',(0.,0.,-1.));
#14589=DIRECTION('ref_axis',(-1.,0.,0.));
#14590=DIRECTION('',(0.,0.,-1.));
#14591=DIRECTION('center_axis',(1.68215601615234E-15,-1.,0.));
#14592=DIRECTION('ref_axis',(1.,1.68215601615234E-15,0.));
#14593=DIRECTION('',(0.,0.,-1.));
#14594=DIRECTION('center_axis',(0.,0.,-1.));
#14595=DIRECTION('ref_axis',(-1.,0.,0.));
#14596=DIRECTION('',(0.,0.,-1.));
#14597=DIRECTION('center_axis',(1.,1.68215592970338E-15,0.));
#14598=DIRECTION('ref_axis',(-1.68215592970338E-15,1.,0.));
#14599=DIRECTION('',(0.,0.,-1.));
#14600=DIRECTION('center_axis',(0.,0.,-1.));
#14601=DIRECTION('ref_axis',(-1.,0.,0.));
#14602=DIRECTION('',(0.,0.,-1.));
#14603=DIRECTION('center_axis',(1.38779120854846E-13,1.,0.));
#14604=DIRECTION('ref_axis',(-1.,1.38779120854846E-13,0.));
#14605=DIRECTION('',(0.,0.,-1.));
#14606=DIRECTION('center_axis',(0.,0.,-1.));
#14607=DIRECTION('ref_axis',(-1.,0.,0.));
#14608=DIRECTION('',(0.,0.,-1.));
#14609=DIRECTION('center_axis',(1.,0.,0.));
#14610=DIRECTION('ref_axis',(0.,0.,-1.));
#14611=DIRECTION('',(0.,0.,-1.));
#14612=DIRECTION('center_axis',(0.,0.,-1.));
#14613=DIRECTION('ref_axis',(-1.,0.,0.));
#14614=DIRECTION('',(0.,0.,-1.));
#14615=DIRECTION('center_axis',(-7.70988123297925E-15,1.,0.));
#14616=DIRECTION('ref_axis',(-1.,-7.70988123297925E-15,0.));
#14617=DIRECTION('',(0.,0.,-1.));
#14618=DIRECTION('center_axis',(0.,0.,-1.));
#14619=DIRECTION('ref_axis',(-1.,0.,0.));
#14620=DIRECTION('',(0.,0.,-1.));
#14621=DIRECTION('center_axis',(-1.,-4.0817021727476E-15,0.));
#14622=DIRECTION('ref_axis',(4.0817021727476E-15,-1.,0.));
#14623=DIRECTION('',(0.,0.,-1.));
#14624=DIRECTION('center_axis',(0.,0.,-1.));
#14625=DIRECTION('ref_axis',(-1.,0.,0.));
#14626=DIRECTION('',(0.,0.,-1.));
#14627=DIRECTION('center_axis',(2.72113516754055E-15,1.,0.));
#14628=DIRECTION('ref_axis',(-1.,2.72113516754055E-15,0.));
#14629=DIRECTION('',(0.,0.,-1.));
#14630=DIRECTION('center_axis',(0.707106781186548,0.707106781186548,0.));
#14631=DIRECTION('ref_axis',(-0.707106781186548,0.707106781186548,0.));
#14632=DIRECTION('',(0.,0.,-1.));
#14633=DIRECTION('center_axis',(1.,0.,0.));
#14634=DIRECTION('ref_axis',(0.,0.,-1.));
#14635=DIRECTION('',(0.,0.,-1.));
#14636=DIRECTION('center_axis',(0.866026135466859,0.499998732686731,0.));
#14637=DIRECTION('ref_axis',(-0.499998732686731,0.866026135466859,0.));
#14638=DIRECTION('',(0.,0.,-1.));
#14639=DIRECTION('center_axis',(0.866026135466859,-0.499998732686731,0.));
#14640=DIRECTION('ref_axis',(0.499998732686731,0.866026135466859,0.));
#14641=DIRECTION('',(0.,0.,-1.));
#14642=DIRECTION('center_axis',(1.,0.,0.));
#14643=DIRECTION('ref_axis',(0.,0.,-1.));
#14644=DIRECTION('',(0.,0.,-1.));
#14645=DIRECTION('center_axis',(0.707106781186548,-0.707106781186547,0.));
#14646=DIRECTION('ref_axis',(0.707106781186547,0.707106781186548,0.));
#14647=DIRECTION('',(0.,0.,-1.));
#14648=DIRECTION('center_axis',(0.,-1.,0.));
#14649=DIRECTION('ref_axis',(0.,0.,-1.));
#14650=DIRECTION('',(0.,0.,-1.));
#14651=DIRECTION('center_axis',(0.,0.,-1.));
#14652=DIRECTION('ref_axis',(-1.,0.,0.));
#14653=DIRECTION('',(0.,0.,-1.));
#14654=DIRECTION('center_axis',(-1.,0.,0.));
#14655=DIRECTION('ref_axis',(0.,0.,1.));
#14656=DIRECTION('',(0.,0.,-1.));
#14657=DIRECTION('center_axis',(0.,0.,-1.));
#14658=DIRECTION('ref_axis',(-1.,0.,0.));
#14659=DIRECTION('',(0.,0.,-1.));
#14660=DIRECTION('center_axis',(7.70988123297925E-15,-1.,0.));
#14661=DIRECTION('ref_axis',(1.,7.70988123297925E-15,0.));
#14662=DIRECTION('',(0.,0.,-1.));
#14663=DIRECTION('center_axis',(0.,0.,-1.));
#14664=DIRECTION('ref_axis',(-1.,0.,0.));
#14665=DIRECTION('',(0.,0.,-1.));
#14666=DIRECTION('center_axis',(1.,0.,0.));
#14667=DIRECTION('ref_axis',(0.,0.,-1.));
#14668=DIRECTION('',(0.,0.,-1.));
#14669=DIRECTION('center_axis',(0.,0.,-1.));
#14670=DIRECTION('ref_axis',(-1.,0.,0.));
#14671=DIRECTION('',(0.,0.,-1.));
#14672=DIRECTION('center_axis',(6.93895604274136E-14,-1.,0.));
#14673=DIRECTION('ref_axis',(1.,6.93895604274136E-14,0.));
#14674=DIRECTION('',(0.,0.,-1.));
#14675=DIRECTION('center_axis',(0.,0.,-1.));
#14676=DIRECTION('ref_axis',(-1.,0.,0.));
#14677=DIRECTION('',(0.,0.,-1.));
#14678=DIRECTION('center_axis',(1.,1.68215592970338E-15,0.));
#14679=DIRECTION('ref_axis',(-1.68215592970338E-15,1.,0.));
#14680=DIRECTION('',(0.,0.,-1.));
#14681=DIRECTION('center_axis',(0.,0.,-1.));
#14682=DIRECTION('ref_axis',(-1.,0.,0.));
#14683=DIRECTION('',(0.,0.,-1.));
#14684=DIRECTION('center_axis',(0.,1.,0.));
#14685=DIRECTION('ref_axis',(0.,0.,1.));
#14686=DIRECTION('',(0.,0.,-1.));
#14687=DIRECTION('center_axis',(0.,0.,-1.));
#14688=DIRECTION('ref_axis',(-1.,0.,0.));
#14689=DIRECTION('',(0.,0.,-1.));
#14690=DIRECTION('center_axis',(-1.,0.,0.));
#14691=DIRECTION('ref_axis',(0.,0.,1.));
#14692=DIRECTION('',(0.,0.,-1.));
#14693=DIRECTION('center_axis',(0.,0.,-1.));
#14694=DIRECTION('ref_axis',(-1.,0.,0.));
#14695=DIRECTION('',(0.,0.,-1.));
#14696=DIRECTION('center_axis',(3.46945490866966E-14,1.,0.));
#14697=DIRECTION('ref_axis',(-1.,3.46945490866966E-14,0.));
#14698=DIRECTION('',(0.,0.,-1.));
#14699=DIRECTION('center_axis',(0.,0.,-1.));
#14700=DIRECTION('ref_axis',(-1.,0.,0.));
#14701=DIRECTION('',(0.,0.,-1.));
#14702=DIRECTION('center_axis',(-1.,-1.54197609341422E-14,0.));
#14703=DIRECTION('ref_axis',(1.54197609341422E-14,-1.,0.));
#14704=DIRECTION('',(0.,0.,-1.));
#14705=DIRECTION('center_axis',(0.,0.,-1.));
#14706=DIRECTION('ref_axis',(-1.,0.,0.));
#14707=DIRECTION('',(0.,0.,-1.));
#14708=DIRECTION('center_axis',(-1.0204256560972E-15,-1.,0.));
#14709=DIRECTION('ref_axis',(1.,-1.0204256560972E-15,0.));
#14710=DIRECTION('',(0.,0.,-1.));
#14711=DIRECTION('center_axis',(0.,0.,-1.));
#14712=DIRECTION('ref_axis',(-1.,0.,0.));
#14713=DIRECTION('',(0.,0.,-1.));
#14714=DIRECTION('center_axis',(-1.,0.,0.));
#14715=DIRECTION('ref_axis',(0.,0.,1.));
#14716=DIRECTION('',(0.,0.,-1.));
#14717=DIRECTION('center_axis',(-0.707496679341793,0.706716667923104,0.));
#14718=DIRECTION('ref_axis',(-0.706716667923105,-0.707496679341793,0.));
#14719=DIRECTION('',(0.,0.,-1.));
#14720=DIRECTION('center_axis',(2.09985316358847E-15,1.,0.));
#14721=DIRECTION('ref_axis',(-1.,2.09985316358847E-15,0.));
#14722=DIRECTION('center_axis',(0.,0.,-1.));
#14723=DIRECTION('ref_axis',(0.707106781186544,0.707106781186551,0.));
#14724=DIRECTION('',(0.,0.,-1.));
#14725=DIRECTION('',(0.,0.,-1.));
#14726=DIRECTION('center_axis',(0.,-1.,0.));
#14727=DIRECTION('ref_axis',(0.,0.,-1.));
#14728=DIRECTION('',(0.,0.,-1.));
#14729=DIRECTION('center_axis',(0.,0.,-1.));
#14730=DIRECTION('ref_axis',(-1.,0.,0.));
#14731=DIRECTION('',(0.,0.,-1.));
#14732=DIRECTION('center_axis',(1.,0.,0.));
#14733=DIRECTION('ref_axis',(0.,0.,-1.));
#14734=DIRECTION('',(0.,0.,-1.));
#14735=DIRECTION('center_axis',(0.,0.,-1.));
#14736=DIRECTION('ref_axis',(-1.,0.,0.));
#14737=DIRECTION('',(0.,0.,-1.));
#14738=DIRECTION('center_axis',(-3.15404158980207E-15,1.,0.));
#14739=DIRECTION('ref_axis',(-1.,-3.15404158980207E-15,0.));
#14740=DIRECTION('',(0.,0.,-1.));
#14741=DIRECTION('center_axis',(0.,0.,-1.));
#14742=DIRECTION('ref_axis',(0.707106781186541,-0.707106781186554,0.));
#14743=DIRECTION('',(0.,0.,-1.));
#14744=DIRECTION('center_axis',(-1.,-6.30808317960405E-15,0.));
#14745=DIRECTION('ref_axis',(6.30808317960405E-15,-1.,0.));
#14746=DIRECTION('center_axis',(0.,0.,-1.));
#14747=DIRECTION('ref_axis',(-1.,0.,0.));
#14748=DIRECTION('',(0.,0.,-1.));
#14749=DIRECTION('',(0.,0.,-1.));
#14750=DIRECTION('center_axis',(-0.627534586286487,-0.778588686672397,0.));
#14751=DIRECTION('ref_axis',(0.778588686672397,-0.627534586286487,0.));
#14752=DIRECTION('',(0.,0.,-1.));
#14753=DIRECTION('center_axis',(0.,0.,-1.));
#14754=DIRECTION('ref_axis',(-1.,0.,0.));
#14755=DIRECTION('',(0.,0.,-1.));
#14756=DIRECTION('center_axis',(0.785495070023503,0.61886791399197,0.));
#14757=DIRECTION('ref_axis',(-0.61886791399197,0.785495070023503,0.));
#14758=DIRECTION('center_axis',(0.785495070023487,-0.61886791399199,0.));
#14759=DIRECTION('ref_axis',(0.61886791399199,0.785495070023487,0.));
#14760=DIRECTION('',(0.,0.,-1.));
#14761=DIRECTION('center_axis',(0.,0.,-1.));
#14762=DIRECTION('ref_axis',(-1.,0.,0.));
#14763=DIRECTION('',(0.,0.,-1.));
#14764=DIRECTION('center_axis',(-0.627534586286517,0.778588686672372,0.));
#14765=DIRECTION('ref_axis',(-0.778588686672372,-0.627534586286517,0.));
#14766=DIRECTION('',(0.,0.,-1.));
#14767=DIRECTION('center_axis',(0.,0.,-1.));
#14768=DIRECTION('ref_axis',(-1.,0.,0.));
#14769=DIRECTION('',(0.,0.,-1.));
#14770=DIRECTION('center_axis',(0.627534586286505,0.778588686672382,0.));
#14771=DIRECTION('ref_axis',(-0.778588686672382,0.627534586286505,0.));
#14772=DIRECTION('',(0.,0.,-1.));
#14773=DIRECTION('center_axis',(0.,0.,-1.));
#14774=DIRECTION('ref_axis',(-1.,0.,0.));
#14775=DIRECTION('',(0.,0.,-1.));
#14776=DIRECTION('center_axis',(-0.785495070023481,-0.618867913991998,0.));
#14777=DIRECTION('ref_axis',(0.618867913991998,-0.785495070023481,0.));
#14778=DIRECTION('',(0.,0.,-1.));
#14779=DIRECTION('center_axis',(0.,0.,-1.));
#14780=DIRECTION('ref_axis',(1.,-3.21624529935327E-16,0.));
#14781=DIRECTION('',(0.,0.,-1.));
#14782=DIRECTION('center_axis',(-0.785495070023503,0.61886791399197,0.));
#14783=DIRECTION('ref_axis',(-0.61886791399197,-0.785495070023503,0.));
#14784=DIRECTION('',(0.,0.,-1.));
#14785=DIRECTION('center_axis',(0.,0.,-1.));
#14786=DIRECTION('ref_axis',(-1.,0.,0.));
#14787=DIRECTION('',(0.,0.,-1.));
#14788=DIRECTION('center_axis',(0.627534586286492,-0.778588686672393,0.));
#14789=DIRECTION('ref_axis',(0.778588686672393,0.627534586286492,0.));
#14790=DIRECTION('center_axis',(0.,0.,-1.));
#14791=DIRECTION('ref_axis',(-1.,0.,0.));
#14792=DIRECTION('',(0.,0.,-1.));
#14793=DIRECTION('',(0.,0.,-1.));
#14794=DIRECTION('center_axis',(0.,1.,0.));
#14795=DIRECTION('ref_axis',(0.,0.,1.));
#14796=DIRECTION('',(0.,0.,-1.));
#14797=DIRECTION('center_axis',(0.,0.,-1.));
#14798=DIRECTION('ref_axis',(0.707106781186549,-0.707106781186546,0.));
#14799=DIRECTION('',(0.,0.,-1.));
#14800=DIRECTION('center_axis',(-1.,0.,0.));
#14801=DIRECTION('ref_axis',(0.,0.,1.));
#14802=DIRECTION('',(0.,0.,-1.));
#14803=DIRECTION('center_axis',(0.,0.,-1.));
#14804=DIRECTION('ref_axis',(0.707106781186547,0.707106781186548,0.));
#14805=DIRECTION('',(0.,0.,-1.));
#14806=DIRECTION('center_axis',(3.15404158980205E-15,-1.,0.));
#14807=DIRECTION('ref_axis',(1.,3.15404158980205E-15,0.));
#14808=DIRECTION('',(0.,0.,-1.));
#14809=DIRECTION('center_axis',(0.,0.,-1.));
#14810=DIRECTION('ref_axis',(-1.,0.,0.));
#14811=DIRECTION('',(0.,0.,-1.));
#14812=DIRECTION('center_axis',(1.,6.30808317960409E-15,0.));
#14813=DIRECTION('ref_axis',(-6.30808317960409E-15,1.,0.));
#14814=DIRECTION('center_axis',(0.,0.,-1.));
#14815=DIRECTION('ref_axis',(0.707106781186549,-0.707106781186546,0.));
#14816=DIRECTION('',(0.,0.,-1.));
#14817=DIRECTION('',(0.,0.,-1.));
#14818=DIRECTION('center_axis',(-1.,-6.30808317960404E-15,0.));
#14819=DIRECTION('ref_axis',(6.30808317960404E-15,-1.,0.));
#14820=DIRECTION('',(0.,0.,-1.));
#14821=DIRECTION('center_axis',(0.,0.,-1.));
#14822=DIRECTION('ref_axis',(0.707106781186541,0.707106781186554,0.));
#14823=DIRECTION('',(0.,0.,-1.));
#14824=DIRECTION('center_axis',(0.,-1.,0.));
#14825=DIRECTION('ref_axis',(0.,0.,-1.));
#14826=DIRECTION('',(0.,0.,-1.));
#14827=DIRECTION('center_axis',(0.,0.,-1.));
#14828=DIRECTION('ref_axis',(-1.,0.,0.));
#14829=DIRECTION('',(0.,0.,-1.));
#14830=DIRECTION('center_axis',(1.,0.,0.));
#14831=DIRECTION('ref_axis',(0.,0.,-1.));
#14832=DIRECTION('',(0.,0.,-1.));
#14833=DIRECTION('center_axis',(0.,0.,-1.));
#14834=DIRECTION('ref_axis',(-1.,0.,0.));
#14835=DIRECTION('',(0.,0.,-1.));
#14836=DIRECTION('center_axis',(-3.15404158980205E-15,1.,0.));
#14837=DIRECTION('ref_axis',(-1.,-3.15404158980205E-15,0.));
#14838=DIRECTION('center_axis',(0.,0.,-1.));
#14839=DIRECTION('ref_axis',(0.707106781186551,0.707106781186544,0.));
#14840=DIRECTION('',(0.,0.,-1.));
#14841=DIRECTION('',(0.,0.,-1.));
#14842=DIRECTION('center_axis',(0.,-1.,0.));
#14843=DIRECTION('ref_axis',(0.,0.,-1.));
#14844=DIRECTION('',(0.,0.,-1.));
#14845=DIRECTION('center_axis',(0.,0.,-1.));
#14846=DIRECTION('ref_axis',(-1.,0.,0.));
#14847=DIRECTION('',(0.,0.,-1.));
#14848=DIRECTION('center_axis',(1.,6.30808317960409E-15,0.));
#14849=DIRECTION('ref_axis',(-6.30808317960409E-15,1.,0.));
#14850=DIRECTION('',(0.,0.,-1.));
#14851=DIRECTION('center_axis',(0.,0.,-1.));
#14852=DIRECTION('ref_axis',(-1.,0.,0.));
#14853=DIRECTION('',(0.,0.,-1.));
#14854=DIRECTION('center_axis',(0.,1.,0.));
#14855=DIRECTION('ref_axis',(0.,0.,1.));
#14856=DIRECTION('',(0.,0.,-1.));
#14857=DIRECTION('center_axis',(0.,0.,-1.));
#14858=DIRECTION('ref_axis',(0.707106781186548,-0.707106781186547,0.));
#14859=DIRECTION('',(0.,0.,-1.));
#14860=DIRECTION('center_axis',(-1.,0.,0.));
#14861=DIRECTION('ref_axis',(0.,0.,1.));
#14862=DIRECTION('axis',(0.,0.,1.));
#14863=DIRECTION('refdir',(1.,0.,0.));
#14864=DIRECTION('center_axis',(-1.,0.,0.));
#14865=DIRECTION('ref_axis',(0.,0.,1.));
#14866=DIRECTION('center_axis',(1.,0.,4.33680868994202E-16));
#14867=DIRECTION('ref_axis',(4.33680868994202E-16,0.,-1.));
#14868=DIRECTION('',(-1.,0.,0.));
#14869=DIRECTION('center_axis',(1.,0.,0.));
#14870=DIRECTION('ref_axis',(0.,0.,1.));
#14871=DIRECTION('center_axis',(-1.,0.,0.));
#14872=DIRECTION('ref_axis',(0.,0.,1.));
#14873=DIRECTION('center_axis',(-1.,0.,0.));
#14874=DIRECTION('ref_axis',(0.,0.,-1.));
#14875=DIRECTION('',(-1.,0.,0.));
#14876=DIRECTION('center_axis',(-1.,0.,0.));
#14877=DIRECTION('ref_axis',(0.,0.,1.));
#14878=DIRECTION('center_axis',(-1.,0.,0.));
#14879=DIRECTION('ref_axis',(0.,0.,1.));
#14880=DIRECTION('',(0.,0.,-1.));
#14881=DIRECTION('',(0.,-1.,0.));
#14882=DIRECTION('',(0.,0.,1.));
#14883=DIRECTION('',(0.,-1.,0.));
#14884=DIRECTION('center_axis',(1.,0.,0.));
#14885=DIRECTION('ref_axis',(0.,0.,1.));
#14886=DIRECTION('center_axis',(-1.,0.,0.));
#14887=DIRECTION('ref_axis',(0.,0.,1.));
#14888=DIRECTION('',(0.,0.,-1.));
#14889=DIRECTION('',(0.,-1.,0.));
#14890=DIRECTION('',(0.,0.,1.));
#14891=DIRECTION('',(0.,-1.,0.));
#14892=DIRECTION('center_axis',(-1.,0.,0.));
#14893=DIRECTION('ref_axis',(0.,0.,1.));
#14894=DIRECTION('center_axis',(-1.,0.,0.));
#14895=DIRECTION('ref_axis',(0.,0.,1.));
#14896=DIRECTION('',(0.,0.,1.));
#14897=DIRECTION('',(0.,-1.,0.));
#14898=DIRECTION('',(0.,0.,-1.));
#14899=DIRECTION('center_axis',(-1.,0.,0.));
#14900=DIRECTION('ref_axis',(0.,0.,1.));
#14901=DIRECTION('',(0.,-1.,0.));
#14902=DIRECTION('center_axis',(0.,0.,-1.));
#14903=DIRECTION('ref_axis',(-1.,0.,0.));
#14904=DIRECTION('',(1.,0.,0.));
#14905=DIRECTION('',(0.,1.,0.));
#14906=DIRECTION('',(1.,0.,0.));
#14907=DIRECTION('',(1.,0.,0.));
#14908=DIRECTION('',(0.,-1.,0.));
#14909=DIRECTION('',(-1.,0.,0.));
#14910=DIRECTION('center_axis',(1.,0.,4.33680868994202E-16));
#14911=DIRECTION('ref_axis',(4.33680868994202E-16,0.,-1.));
#14912=DIRECTION('center_axis',(1.,0.,4.33680868994202E-16));
#14913=DIRECTION('ref_axis',(4.33680868994202E-16,0.,-1.));
#14914=DIRECTION('',(-4.33680868994202E-16,0.,1.));
#14915=DIRECTION('',(0.,1.,0.));
#14916=DIRECTION('',(-4.33680868994202E-16,0.,1.));
#14917=DIRECTION('center_axis',(1.,0.,4.33680868994202E-16));
#14918=DIRECTION('ref_axis',(4.33680868994202E-16,0.,-1.));
#14919=DIRECTION('center_axis',(1.73472347597681E-16,0.,1.));
#14920=DIRECTION('ref_axis',(1.,0.,-1.73472347597681E-16));
#14921=DIRECTION('',(-1.,0.,1.73472347597681E-16));
#14922=DIRECTION('',(0.,1.,0.));
#14923=DIRECTION('',(1.,0.,0.));
#14924=DIRECTION('',(0.,1.,0.));
#14925=DIRECTION('',(-1.,0.,0.));
#14926=DIRECTION('',(0.,1.,0.));
#14927=DIRECTION('',(-1.,0.,1.73472347597681E-16));
#14928=DIRECTION('',(0.,-1.,0.));
#14929=DIRECTION('center_axis',(-1.,0.,0.));
#14930=DIRECTION('ref_axis',(0.,0.,1.));
#14931=DIRECTION('',(0.,0.,1.));
#14932=DIRECTION('',(0.,-1.,0.));
#14933=DIRECTION('',(0.,0.,-1.));
#14934=DIRECTION('center_axis',(1.,0.,0.));
#14935=DIRECTION('ref_axis',(0.,0.,1.));
#14936=DIRECTION('',(0.,-1.,0.));
#14937=DIRECTION('center_axis',(0.,0.,1.));
#14938=DIRECTION('ref_axis',(1.,0.,0.));
#14939=DIRECTION('',(0.,-1.,0.));
#14940=DIRECTION('',(1.,0.,0.));
#14941=DIRECTION('',(-1.,0.,0.));
#14942=DIRECTION('',(0.,1.,0.));
#14943=DIRECTION('',(-1.,0.,0.));
#14944=DIRECTION('',(-1.,0.,0.));
#14945=DIRECTION('center_axis',(-1.,0.,0.));
#14946=DIRECTION('ref_axis',(0.,0.,1.));
#14947=DIRECTION('',(0.,0.,-1.));
#14948=DIRECTION('center_axis',(-1.,0.,0.));
#14949=DIRECTION('ref_axis',(0.,0.,1.));
#14950=DIRECTION('center_axis',(-1.,0.,0.));
#14951=DIRECTION('ref_axis',(0.,0.,1.));
#14952=DIRECTION('',(0.,0.,-1.));
#14953=DIRECTION('',(0.,1.,0.));
#14954=DIRECTION('center_axis',(0.,0.,1.));
#14955=DIRECTION('ref_axis',(1.,0.,0.));
#14956=DIRECTION('',(-1.,0.,0.));
#14957=DIRECTION('',(0.,1.,0.));
#14958=DIRECTION('',(-1.,0.,-7.2280144832367E-17));
#14959=DIRECTION('',(0.,1.,0.));
#14960=DIRECTION('',(1.,0.,7.2280144832367E-17));
#14961=DIRECTION('',(0.,1.,0.));
#14962=DIRECTION('',(-1.,0.,0.));
#14963=DIRECTION('',(0.,-1.,0.));
#14964=DIRECTION('center_axis',(0.,1.,0.));
#14965=DIRECTION('ref_axis',(0.,0.,1.));
#14966=DIRECTION('center_axis',(0.,1.,0.));
#14967=DIRECTION('ref_axis',(0.,0.,1.));
#14968=DIRECTION('',(1.,0.,0.));
#14969=DIRECTION('center_axis',(0.,-1.,0.));
#14970=DIRECTION('ref_axis',(0.,0.,1.));
#14971=DIRECTION('center_axis',(0.,1.,0.));
#14972=DIRECTION('ref_axis',(0.,0.,1.));
#14973=DIRECTION('',(-1.,0.,0.));
#14974=DIRECTION('center_axis',(0.,-1.,0.));
#14975=DIRECTION('ref_axis',(0.,0.,1.));
#14976=DIRECTION('center_axis',(0.,1.,0.));
#14977=DIRECTION('ref_axis',(0.,0.,1.));
#14978=DIRECTION('',(-1.,0.,2.16840434497101E-16));
#14979=DIRECTION('center_axis',(0.,1.,0.));
#14980=DIRECTION('ref_axis',(0.,0.,1.));
#14981=DIRECTION('',(1.,0.,-2.16840434497101E-16));
#14982=DIRECTION('center_axis',(0.,1.,0.));
#14983=DIRECTION('ref_axis',(0.,0.,1.));
#14984=DIRECTION('center_axis',(0.,-1.,0.));
#14985=DIRECTION('ref_axis',(0.,0.,1.));
#14986=DIRECTION('center_axis',(0.,1.,0.));
#14987=DIRECTION('ref_axis',(0.,0.,1.));
#14988=DIRECTION('',(1.,0.,0.));
#14989=DIRECTION('center_axis',(0.,-1.,0.));
#14990=DIRECTION('ref_axis',(0.,0.,1.));
#14991=DIRECTION('center_axis',(0.,1.,0.));
#14992=DIRECTION('ref_axis',(0.,0.,1.));
#14993=DIRECTION('',(-1.,0.,0.));
#14994=DIRECTION('',(-1.,0.,2.16840434497101E-16));
#14995=DIRECTION('center_axis',(0.,1.,0.));
#14996=DIRECTION('ref_axis',(0.,0.,1.));
#14997=DIRECTION('',(1.,0.,-2.16840434497101E-16));
#14998=DIRECTION('center_axis',(0.,1.,0.));
#14999=DIRECTION('ref_axis',(0.,0.,1.));
#15000=DIRECTION('center_axis',(0.,1.,0.));
#15001=DIRECTION('ref_axis',(0.,0.,1.));
#15002=DIRECTION('',(0.,1.,0.));
#15003=DIRECTION('',(0.,1.,0.));
#15004=DIRECTION('center_axis',(-2.16840434497101E-16,0.,-1.));
#15005=DIRECTION('ref_axis',(-1.,0.,2.16840434497101E-16));
#15006=DIRECTION('',(0.,1.,0.));
#15007=DIRECTION('center_axis',(0.,1.,0.));
#15008=DIRECTION('ref_axis',(0.,0.,1.));
#15009=DIRECTION('',(0.,1.,0.));
#15010=DIRECTION('center_axis',(2.16840434497101E-16,0.,1.));
#15011=DIRECTION('ref_axis',(1.,0.,-2.16840434497101E-16));
#15012=DIRECTION('center_axis',(0.,-1.,0.));
#15013=DIRECTION('ref_axis',(0.,0.,-1.));
#15014=DIRECTION('center_axis',(0.,1.,0.));
#15015=DIRECTION('ref_axis',(0.,0.,1.));
#15016=DIRECTION('center_axis',(1.,0.,0.));
#15017=DIRECTION('ref_axis',(0.,0.,-1.));
#15018=DIRECTION('center_axis',(-1.,0.,0.));
#15019=DIRECTION('ref_axis',(0.,0.,1.));
#15020=DIRECTION('center_axis',(1.,0.,0.));
#15021=DIRECTION('ref_axis',(0.,0.,-1.));
#15022=DIRECTION('center_axis',(-1.,0.,0.));
#15023=DIRECTION('ref_axis',(0.,0.,1.));
#15024=DIRECTION('center_axis',(0.,1.,0.));
#15025=DIRECTION('ref_axis',(0.,0.,1.));
#15026=DIRECTION('center_axis',(0.,-1.,0.));
#15027=DIRECTION('ref_axis',(0.,0.,1.));
#15028=DIRECTION('center_axis',(0.,1.,0.));
#15029=DIRECTION('ref_axis',(0.,0.,1.));
#15030=DIRECTION('',(0.,0.,1.));
#15031=DIRECTION('center_axis',(0.,1.,0.));
#15032=DIRECTION('ref_axis',(0.,0.,1.));
#15033=DIRECTION('',(0.,0.,1.));
#15034=DIRECTION('center_axis',(0.,-1.,0.));
#15035=DIRECTION('ref_axis',(0.,0.,1.));
#15036=DIRECTION('center_axis',(0.,1.,0.));
#15037=DIRECTION('ref_axis',(0.,0.,1.));
#15038=DIRECTION('center_axis',(-1.,0.,0.));
#15039=DIRECTION('ref_axis',(0.,0.,1.));
#15040=DIRECTION('',(0.,-1.,0.));
#15041=DIRECTION('center_axis',(0.,-1.,0.));
#15042=DIRECTION('ref_axis',(0.,0.,-1.));
#15043=DIRECTION('center_axis',(0.,-1.,0.));
#15044=DIRECTION('ref_axis',(0.,0.,-1.));
#15045=DIRECTION('center_axis',(0.,1.,0.));
#15046=DIRECTION('ref_axis',(0.,0.,-1.));
#15047=DIRECTION('',(0.,0.,1.));
#15048=DIRECTION('center_axis',(0.,-1.,0.));
#15049=DIRECTION('ref_axis',(0.,0.,-1.));
#15050=DIRECTION('',(0.,0.,1.));
#15051=DIRECTION('center_axis',(0.,-1.,0.));
#15052=DIRECTION('ref_axis',(0.,0.,-1.));
#15053=DIRECTION('center_axis',(0.,1.,0.));
#15054=DIRECTION('ref_axis',(0.,0.,-1.));
#15055=DIRECTION('center_axis',(1.,0.,0.));
#15056=DIRECTION('ref_axis',(0.,0.,-1.));
#15057=DIRECTION('',(0.,-1.,0.));
#15058=DIRECTION('center_axis',(0.,-1.,0.));
#15059=DIRECTION('ref_axis',(0.,0.,-1.));
#15060=DIRECTION('center_axis',(0.,-1.,0.));
#15061=DIRECTION('ref_axis',(0.,0.,-1.));
#15062=DIRECTION('center_axis',(0.,-1.,0.));
#15063=DIRECTION('ref_axis',(0.,0.,-1.));
#15064=DIRECTION('center_axis',(0.,1.,0.));
#15065=DIRECTION('ref_axis',(0.,0.,1.));
#15066=DIRECTION('center_axis',(0.,1.,0.));
#15067=DIRECTION('ref_axis',(0.,0.,1.));
#15068=DIRECTION('center_axis',(0.,1.,0.));
#15069=DIRECTION('ref_axis',(0.,0.,1.));
#15070=DIRECTION('axis',(0.,0.,1.));
#15071=DIRECTION('refdir',(1.,0.,0.));
#15072=DIRECTION('center_axis',(0.,0.,1.));
#15073=DIRECTION('ref_axis',(1.,0.,0.));
#15074=DIRECTION('center_axis',(0.,0.,1.));
#15075=DIRECTION('ref_axis',(1.,0.,0.));
#15076=DIRECTION('',(0.,0.,1.));
#15077=DIRECTION('center_axis',(0.,0.,1.));
#15078=DIRECTION('ref_axis',(1.,0.,0.));
#15079=DIRECTION('center_axis',(0.,0.,1.));
#15080=DIRECTION('ref_axis',(1.,0.,0.));
#15081=DIRECTION('center_axis',(0.,0.,1.));
#15082=DIRECTION('ref_axis',(1.,0.,0.));
#15083=DIRECTION('',(0.,0.,1.));
#15084=DIRECTION('center_axis',(0.,0.,1.));
#15085=DIRECTION('ref_axis',(1.,0.,0.));
#15086=DIRECTION('center_axis',(0.,0.,1.));
#15087=DIRECTION('ref_axis',(1.,0.,0.));
#15088=DIRECTION('',(0.,-1.,0.));
#15089=DIRECTION('center_axis',(0.,0.,-1.));
#15090=DIRECTION('ref_axis',(1.,0.,0.));
#15091=DIRECTION('',(-1.,0.,0.));
#15092=DIRECTION('center_axis',(0.,0.,-1.));
#15093=DIRECTION('ref_axis',(1.,2.60208521396521E-15,0.));
#15094=DIRECTION('',(0.,1.,0.));
#15095=DIRECTION('',(1.,-1.73472347597681E-16,0.));
#15096=DIRECTION('center_axis',(0.,0.,1.));
#15097=DIRECTION('ref_axis',(1.,0.,0.));
#15098=DIRECTION('',(-1.,0.,0.));
#15099=DIRECTION('',(0.,1.,0.));
#15100=DIRECTION('',(1.,1.73472347597681E-16,0.));
#15101=DIRECTION('',(-8.67361737988404E-17,1.,0.));
#15102=DIRECTION('',(1.,0.,1.26217744835362E-26));
#15103=DIRECTION('',(-8.67361737988404E-17,1.,0.));
#15104=DIRECTION('',(1.,1.73472347597681E-16,0.));
#15105=DIRECTION('',(0.,-1.,0.));
#15106=DIRECTION('center_axis',(-1.73472347597681E-16,1.,0.));
#15107=DIRECTION('ref_axis',(-1.,-1.73472347597681E-16,0.));
#15108=DIRECTION('',(0.,0.,-1.));
#15109=DIRECTION('',(1.,1.73472347597681E-16,0.));
#15110=DIRECTION('',(0.,0.,-1.));
#15111=DIRECTION('center_axis',(-1.73472347597681E-16,1.,0.));
#15112=DIRECTION('ref_axis',(-1.,-1.73472347597681E-16,0.));
#15113=DIRECTION('',(0.,0.,1.));
#15114=DIRECTION('',(0.,0.,-1.));
#15115=DIRECTION('',(1.,1.73472347597681E-16,0.));
#15116=DIRECTION('center_axis',(1.,0.,0.));
#15117=DIRECTION('ref_axis',(0.,0.,-1.));
#15118=DIRECTION('',(0.,-1.,0.));
#15119=DIRECTION('',(0.,0.,-1.));
#15120=DIRECTION('',(0.,0.,1.));
#15121=DIRECTION('',(0.,1.,0.));
#15122=DIRECTION('',(0.,0.,1.));
#15123=DIRECTION('center_axis',(-1.,0.,0.));
#15124=DIRECTION('ref_axis',(0.,0.,1.));
#15125=DIRECTION('',(0.,0.,1.));
#15126=DIRECTION('',(0.,1.,0.));
#15127=DIRECTION('',(0.,0.,1.));
#15128=DIRECTION('',(-2.19585250123647E-16,-1.,0.));
#15129=DIRECTION('',(0.,0.,1.));
#15130=DIRECTION('center_axis',(0.,-1.,0.));
#15131=DIRECTION('ref_axis',(0.,0.,-1.));
#15132=DIRECTION('',(0.,0.,1.));
#15133=DIRECTION('',(-1.,0.,0.));
#15134=DIRECTION('',(0.,0.,-1.));
#15135=DIRECTION('center_axis',(0.,0.,1.));
#15136=DIRECTION('ref_axis',(1.,0.,0.));
#15137=DIRECTION('center_axis',(0.,0.,1.));
#15138=DIRECTION('ref_axis',(1.,0.,0.));
#15139=DIRECTION('',(-8.67361737988404E-17,1.,0.));
#15140=DIRECTION('',(-1.,0.,0.));
#15141=DIRECTION('',(-8.67361737988404E-17,1.,0.));
#15142=DIRECTION('center_axis',(0.,0.,1.));
#15143=DIRECTION('ref_axis',(1.,0.,0.));
#15144=DIRECTION('center_axis',(1.,8.67361737988403E-17,0.));
#15145=DIRECTION('ref_axis',(-8.67361737988404E-17,1.,0.));
#15146=DIRECTION('',(0.,0.,-1.));
#15147=DIRECTION('center_axis',(-1.,-8.67361737988403E-17,0.));
#15148=DIRECTION('ref_axis',(8.67361737988404E-17,-1.,0.));
#15149=DIRECTION('',(0.,0.,1.));
#15150=DIRECTION('center_axis',(0.,-1.,0.));
#15151=DIRECTION('ref_axis',(0.,0.,-1.));
#15152=DIRECTION('center_axis',(0.,1.,0.));
#15153=DIRECTION('ref_axis',(0.,0.,1.));
#15154=DIRECTION('',(-1.,0.,0.));
#15155=DIRECTION('center_axis',(-1.73472347597681E-16,-1.,0.));
#15156=DIRECTION('ref_axis',(1.,-1.73472347597681E-16,0.));
#15157=DIRECTION('',(1.,-1.73472347597681E-16,0.));
#15158=DIRECTION('center_axis',(0.,0.,-1.));
#15159=DIRECTION('ref_axis',(-1.,0.,0.));
#15160=DIRECTION('center_axis',(0.,0.,-1.));
#15161=DIRECTION('ref_axis',(-1.,0.,0.));
#15162=DIRECTION('center_axis',(0.,0.,-1.));
#15163=DIRECTION('ref_axis',(-1.,0.,0.));
#15164=DIRECTION('center_axis',(0.,0.,-1.));
#15165=DIRECTION('ref_axis',(-1.,0.,0.));
#15166=DIRECTION('axis',(0.,0.,1.));
#15167=DIRECTION('refdir',(1.,0.,0.));
#15168=DIRECTION('center_axis',(0.,1.,0.));
#15169=DIRECTION('ref_axis',(0.,0.,1.));
#15170=DIRECTION('',(-1.,0.,1.15648231731787E-16));
#15171=DIRECTION('center_axis',(0.,1.,0.));
#15172=DIRECTION('ref_axis',(0.,0.,1.));
#15173=DIRECTION('',(0.,0.,1.));
#15174=DIRECTION('center_axis',(0.,1.,0.));
#15175=DIRECTION('ref_axis',(0.,0.,1.));
#15176=DIRECTION('',(1.,0.,-1.15648231731787E-16));
#15177=DIRECTION('center_axis',(0.,1.,0.));
#15178=DIRECTION('ref_axis',(0.,0.,1.));
#15179=DIRECTION('',(0.,0.,-1.));
#15180=DIRECTION('center_axis',(0.,1.,0.));
#15181=DIRECTION('ref_axis',(0.,0.,1.));
#15182=DIRECTION('',(1.,0.,-1.03257349760524E-16));
#15183=DIRECTION('',(0.,0.,1.));
#15184=DIRECTION('',(-1.,0.,1.03257349760524E-16));
#15185=DIRECTION('',(0.,0.,-1.));
#15186=DIRECTION('center_axis',(0.,1.,0.));
#15187=DIRECTION('ref_axis',(0.,0.,1.));
#15188=DIRECTION('',(0.,0.,1.));
#15189=DIRECTION('center_axis',(0.,-1.,0.));
#15190=DIRECTION('ref_axis',(0.,0.,1.));
#15191=DIRECTION('',(-1.,0.,1.15648231731787E-16));
#15192=DIRECTION('center_axis',(0.,-1.,0.));
#15193=DIRECTION('ref_axis',(0.,0.,1.));
#15194=DIRECTION('',(0.,0.,-1.));
#15195=DIRECTION('center_axis',(0.,-1.,0.));
#15196=DIRECTION('ref_axis',(0.,0.,1.));
#15197=DIRECTION('',(1.,0.,-1.15648231731787E-16));
#15198=DIRECTION('center_axis',(0.,-1.,0.));
#15199=DIRECTION('ref_axis',(0.,0.,1.));
#15200=DIRECTION('',(0.,0.,1.));
#15201=DIRECTION('',(1.,0.,-1.03257349760524E-16));
#15202=DIRECTION('',(0.,0.,-1.));
#15203=DIRECTION('',(-1.,0.,1.03257349760524E-16));
#15204=DIRECTION('center_axis',(1.,0.,0.));
#15205=DIRECTION('ref_axis',(0.,0.,-1.));
#15206=DIRECTION('',(0.,-1.,0.));
#15207=DIRECTION('',(0.,1.,0.));
#15208=DIRECTION('center_axis',(-1.15648231731787E-16,0.,-1.));
#15209=DIRECTION('ref_axis',(-1.,0.,1.15648231731787E-16));
#15210=DIRECTION('',(0.,-1.,0.));
#15211=DIRECTION('',(0.,1.,0.));
#15212=DIRECTION('center_axis',(-1.,0.,0.));
#15213=DIRECTION('ref_axis',(0.,0.,1.));
#15214=DIRECTION('',(0.,1.,0.));
#15215=DIRECTION('',(0.,-1.,0.));
#15216=DIRECTION('center_axis',(1.15648231731787E-16,0.,1.));
#15217=DIRECTION('ref_axis',(1.,0.,-1.15648231731787E-16));
#15218=DIRECTION('',(0.,1.,0.));
#15219=DIRECTION('',(0.,-1.,0.));
#15220=DIRECTION('center_axis',(1.,0.,0.));
#15221=DIRECTION('ref_axis',(0.,0.,-1.));
#15222=DIRECTION('',(0.,-1.,0.));
#15223=DIRECTION('',(0.,-1.,0.));
#15224=DIRECTION('center_axis',(-1.03257349760524E-16,0.,-1.));
#15225=DIRECTION('ref_axis',(-1.,0.,1.03257349760524E-16));
#15226=DIRECTION('',(0.,-1.,0.));
#15227=DIRECTION('center_axis',(-1.,0.,0.));
#15228=DIRECTION('ref_axis',(0.,0.,1.));
#15229=DIRECTION('',(0.,-1.,0.));
#15230=DIRECTION('center_axis',(1.03257349760524E-16,0.,1.));
#15231=DIRECTION('ref_axis',(1.,0.,-1.03257349760524E-16));
#15232=DIRECTION('center_axis',(0.,-1.,0.));
#15233=DIRECTION('ref_axis',(0.,0.,-1.));
#15234=DIRECTION('center_axis',(0.,-1.,0.));
#15235=DIRECTION('ref_axis',(0.,0.,-1.));
#15236=DIRECTION('center_axis',(0.,-1.,0.));
#15237=DIRECTION('ref_axis',(0.,0.,-1.));
#15238=DIRECTION('center_axis',(0.,-1.,0.));
#15239=DIRECTION('ref_axis',(0.,0.,-1.));
#15240=DIRECTION('axis',(0.,0.,1.));
#15241=DIRECTION('refdir',(1.,0.,0.));
#15242=DIRECTION('center_axis',(0.,0.,1.));
#15243=DIRECTION('ref_axis',(1.,0.,0.));
#15244=DIRECTION('center_axis',(0.,0.,1.));
#15245=DIRECTION('ref_axis',(1.,0.,0.));
#15246=DIRECTION('',(0.,0.,1.));
#15247=DIRECTION('center_axis',(0.,0.,1.));
#15248=DIRECTION('ref_axis',(1.,0.,0.));
#15249=DIRECTION('center_axis',(0.,0.,1.));
#15250=DIRECTION('ref_axis',(1.,0.,0.));
#15251=DIRECTION('center_axis',(0.,0.,1.));
#15252=DIRECTION('ref_axis',(1.,0.,0.));
#15253=DIRECTION('center_axis',(0.,0.,1.));
#15254=DIRECTION('ref_axis',(1.,0.,0.));
#15255=DIRECTION('',(0.0194407696462631,2.38080763202572E-18,-0.999811010379242));
#15256=DIRECTION('center_axis',(0.,0.,1.));
#15257=DIRECTION('ref_axis',(1.,0.,0.));
#15258=DIRECTION('center_axis',(0.,0.,-1.));
#15259=DIRECTION('ref_axis',(-1.,0.,0.));
#15260=DIRECTION('',(-0.0194407696462629,2.38080763202569E-18,0.999811010379242));
#15261=DIRECTION('center_axis',(0.,0.,1.));
#15262=DIRECTION('ref_axis',(1.,0.,0.));
#15263=DIRECTION('center_axis',(0.,0.,1.));
#15264=DIRECTION('ref_axis',(1.,0.,0.));
#15265=DIRECTION('center_axis',(0.,0.,1.));
#15266=DIRECTION('ref_axis',(1.,0.,0.));
#15267=DIRECTION('',(0.,0.,-1.));
#15268=DIRECTION('center_axis',(0.,0.,1.));
#15269=DIRECTION('ref_axis',(1.,0.,0.));
#15270=DIRECTION('center_axis',(0.,0.,-1.));
#15271=DIRECTION('ref_axis',(-1.,0.,0.));
#15272=DIRECTION('center_axis',(0.,0.,1.));
#15273=DIRECTION('ref_axis',(1.,0.,0.));
#15274=DIRECTION('',(0.,0.,1.));
#15275=DIRECTION('center_axis',(0.,0.,1.));
#15276=DIRECTION('ref_axis',(1.,0.,0.));
#15277=DIRECTION('center_axis',(0.,0.,-1.));
#15278=DIRECTION('ref_axis',(-1.,0.,0.));
#15279=DIRECTION('center_axis',(0.,0.,1.));
#15280=DIRECTION('ref_axis',(1.,0.,0.));
#15281=DIRECTION('',(0.,0.,-1.));
#15282=DIRECTION('center_axis',(0.,0.,1.));
#15283=DIRECTION('ref_axis',(1.,0.,0.));
#15284=DIRECTION('center_axis',(0.,0.,-1.));
#15285=DIRECTION('ref_axis',(-1.,0.,0.));
#15286=DIRECTION('center_axis',(0.,0.,1.));
#15287=DIRECTION('ref_axis',(1.,0.,0.));
#15288=DIRECTION('',(0.,0.,-1.));
#15289=DIRECTION('center_axis',(0.,0.,-1.));
#15290=DIRECTION('ref_axis',(-1.,0.,0.));
#15291=DIRECTION('center_axis',(0.,0.,1.));
#15292=DIRECTION('ref_axis',(1.,0.,0.));
#15293=DIRECTION('center_axis',(0.,0.,1.));
#15294=DIRECTION('ref_axis',(1.,0.,0.));
#15295=DIRECTION('center_axis',(0.,0.,1.));
#15296=DIRECTION('ref_axis',(1.,0.,0.));
#15297=DIRECTION('center_axis',(0.,0.,-1.));
#15298=DIRECTION('ref_axis',(1.,0.,0.));
#15299=DIRECTION('center_axis',(0.,0.,-1.));
#15300=DIRECTION('ref_axis',(-1.,0.,0.));
#15301=DIRECTION('center_axis',(0.,0.,1.));
#15302=DIRECTION('ref_axis',(1.,0.,0.));
#15303=DIRECTION('axis',(0.,0.,1.));
#15304=DIRECTION('refdir',(1.,0.,0.));
#15305=DIRECTION('center_axis',(0.,0.,-1.));
#15306=DIRECTION('ref_axis',(0.,1.,0.));
#15307=DIRECTION('center_axis',(-1.,0.,0.));
#15308=DIRECTION('ref_axis',(0.,-1.,0.));
#15309=DIRECTION('center_axis',(0.,1.1188944566643E-16,-1.));
#15310=DIRECTION('ref_axis',(0.,1.,0.));
#15311=DIRECTION('center_axis',(-1.,0.,0.));
#15312=DIRECTION('ref_axis',(0.,-1.,0.));
#15313=DIRECTION('center_axis',(0.,0.,-1.));
#15314=DIRECTION('ref_axis',(0.,1.,0.));
#15315=DIRECTION('center_axis',(-1.,0.,0.));
#15316=DIRECTION('ref_axis',(0.,-1.,0.));
#15317=DIRECTION('center_axis',(0.,0.,-1.));
#15318=DIRECTION('ref_axis',(0.,1.,0.));
#15319=DIRECTION('center_axis',(-1.,0.,0.));
#15320=DIRECTION('ref_axis',(0.,-1.,0.));
#15321=DIRECTION('center_axis',(0.,1.1188944566643E-16,-1.));
#15322=DIRECTION('ref_axis',(0.,1.,0.));
#15323=DIRECTION('center_axis',(-1.,0.,0.));
#15324=DIRECTION('ref_axis',(0.,-1.,0.));
#15325=DIRECTION('center_axis',(0.,0.,-1.));
#15326=DIRECTION('ref_axis',(0.,1.,0.));
#15327=DIRECTION('center_axis',(-1.,0.,0.));
#15328=DIRECTION('ref_axis',(0.,-1.,0.));
#15329=DIRECTION('center_axis',(0.,0.,-1.));
#15330=DIRECTION('ref_axis',(0.,1.,0.));
#15331=DIRECTION('center_axis',(-1.,0.,0.));
#15332=DIRECTION('ref_axis',(0.,-1.,0.));
#15333=DIRECTION('center_axis',(1.,0.,0.));
#15334=DIRECTION('ref_axis',(0.,0.,1.));
#15335=DIRECTION('center_axis',(1.,0.,0.));
#15336=DIRECTION('ref_axis',(0.,0.,1.));
#15337=DIRECTION('center_axis',(0.,1.,1.22464679914735E-16));
#15338=DIRECTION('ref_axis',(0.,1.22464679914735E-16,-1.));
#15339=DIRECTION('center_axis',(1.,0.,0.));
#15340=DIRECTION('ref_axis',(0.,0.,1.));
#15341=DIRECTION('center_axis',(1.,0.,0.));
#15342=DIRECTION('ref_axis',(0.,0.,1.));
#15343=DIRECTION('center_axis',(1.,0.,0.));
#15344=DIRECTION('ref_axis',(0.,0.,1.));
#15345=DIRECTION('',(-1.,0.,0.));
#15346=DIRECTION('center_axis',(1.,0.,0.));
#15347=DIRECTION('ref_axis',(0.,0.,1.));
#15348=DIRECTION('center_axis',(1.,0.,0.));
#15349=DIRECTION('ref_axis',(0.,0.,1.));
#15350=DIRECTION('center_axis',(0.,1.,1.22464679914735E-16));
#15351=DIRECTION('ref_axis',(0.,1.22464679914735E-16,-1.));
#15352=DIRECTION('center_axis',(1.,0.,0.));
#15353=DIRECTION('ref_axis',(0.,0.,1.));
#15354=DIRECTION('center_axis',(1.,0.,0.));
#15355=DIRECTION('ref_axis',(0.,0.,1.));
#15356=DIRECTION('',(1.,0.,0.));
#15357=DIRECTION('center_axis',(1.,0.,0.));
#15358=DIRECTION('ref_axis',(0.,0.,1.));
#15359=DIRECTION('center_axis',(1.,0.,0.));
#15360=DIRECTION('ref_axis',(0.,0.,1.));
#15361=DIRECTION('center_axis',(1.,0.,0.));
#15362=DIRECTION('ref_axis',(0.,0.,1.));
#15363=DIRECTION('center_axis',(0.,-1.,-1.22464679914735E-16));
#15364=DIRECTION('ref_axis',(0.,1.22464679914735E-16,-1.));
#15365=DIRECTION('center_axis',(1.,0.,0.));
#15366=DIRECTION('ref_axis',(0.,0.,1.));
#15367=DIRECTION('center_axis',(1.,0.,0.));
#15368=DIRECTION('ref_axis',(0.,0.,1.));
#15369=DIRECTION('',(0.173648177666934,1.2060416625019E-16,-0.984807753012207));
#15370=DIRECTION('center_axis',(1.,0.,0.));
#15371=DIRECTION('ref_axis',(0.,0.,1.));
#15372=DIRECTION('center_axis',(1.,0.,0.));
#15373=DIRECTION('ref_axis',(0.,0.,1.));
#15374=DIRECTION('',(1.,0.,0.));
#15375=DIRECTION('center_axis',(1.,0.,0.));
#15376=DIRECTION('ref_axis',(0.,0.,1.));
#15377=DIRECTION('center_axis',(1.,0.,0.));
#15378=DIRECTION('ref_axis',(0.,0.,1.));
#15379=DIRECTION('center_axis',(0.,-1.,-1.22464679914735E-16));
#15380=DIRECTION('ref_axis',(0.,1.22464679914735E-16,-1.));
#15381=DIRECTION('center_axis',(1.,0.,0.));
#15382=DIRECTION('ref_axis',(0.,0.,1.));
#15383=DIRECTION('center_axis',(1.,0.,0.));
#15384=DIRECTION('ref_axis',(0.,0.,1.));
#15385=DIRECTION('center_axis',(1.,0.,0.));
#15386=DIRECTION('ref_axis',(0.,0.,1.));
#15387=DIRECTION('',(1.,0.,0.));
#15388=DIRECTION('center_axis',(-1.,0.,0.));
#15389=DIRECTION('ref_axis',(0.,0.,-1.));
#15390=DIRECTION('',(-0.173648177666924,1.2060416625019E-16,0.984807753012209));
#15391=DIRECTION('center_axis',(1.,0.,0.));
#15392=DIRECTION('ref_axis',(0.,0.,1.));
#15393=DIRECTION('center_axis',(1.,0.,0.));
#15394=DIRECTION('ref_axis',(0.,0.,1.));
#15395=DIRECTION('center_axis',(1.,0.,0.));
#15396=DIRECTION('ref_axis',(0.,0.,1.));
#15397=DIRECTION('center_axis',(1.,0.,0.));
#15398=DIRECTION('ref_axis',(0.,0.,1.));
#15399=DIRECTION('center_axis',(0.,-1.,-1.22464679914735E-16));
#15400=DIRECTION('ref_axis',(0.,1.22464679914735E-16,-1.));
#15401=DIRECTION('center_axis',(1.,0.,0.));
#15402=DIRECTION('ref_axis',(0.,0.,1.));
#15403=DIRECTION('center_axis',(1.,0.,0.));
#15404=DIRECTION('ref_axis',(0.,0.,1.));
#15405=DIRECTION('',(1.,0.,0.));
#15406=DIRECTION('center_axis',(-1.,0.,0.));
#15407=DIRECTION('ref_axis',(0.,0.,-1.));
#15408=DIRECTION('center_axis',(1.,0.,0.));
#15409=DIRECTION('ref_axis',(0.,-1.,0.));
#15410=DIRECTION('center_axis',(1.,0.,0.));
#15411=DIRECTION('ref_axis',(0.,0.,1.));
#15412=DIRECTION('center_axis',(1.,0.,0.));
#15413=DIRECTION('ref_axis',(0.,0.,1.));
#15414=DIRECTION('center_axis',(0.,-1.,-1.22464679914735E-16));
#15415=DIRECTION('ref_axis',(0.,1.22464679914735E-16,-1.));
#15416=DIRECTION('center_axis',(1.,0.,0.));
#15417=DIRECTION('ref_axis',(0.,0.,1.));
#15418=DIRECTION('center_axis',(1.,0.,0.));
#15419=DIRECTION('ref_axis',(0.,0.,1.));
#15420=DIRECTION('center_axis',(1.,0.,0.));
#15421=DIRECTION('ref_axis',(0.,0.,1.));
#15422=DIRECTION('',(-0.101599191217213,-1.21830975896784E-16,0.994825414001878));
#15423=DIRECTION('center_axis',(1.,0.,0.));
#15424=DIRECTION('ref_axis',(0.,0.,1.));
#15425=DIRECTION('center_axis',(1.,0.,0.));
#15426=DIRECTION('ref_axis',(0.,0.,1.));
#15427=DIRECTION('center_axis',(1.,0.,0.));
#15428=DIRECTION('ref_axis',(0.,0.,1.));
#15429=DIRECTION('',(-1.,0.,0.));
#15430=DIRECTION('center_axis',(1.,0.,0.));
#15431=DIRECTION('ref_axis',(0.,0.,1.));
#15432=DIRECTION('center_axis',(1.,0.,0.));
#15433=DIRECTION('ref_axis',(0.,0.,1.));
#15434=DIRECTION('center_axis',(1.,0.,0.));
#15435=DIRECTION('ref_axis',(0.,0.,1.));
#15436=DIRECTION('',(0.0509973848574056,1.22305327255588E-16,-0.998698786790945));
#15437=DIRECTION('center_axis',(-1.,0.,0.));
#15438=DIRECTION('ref_axis',(0.,0.,-1.));
#15439=DIRECTION('',(0.0509973848574056,-1.22305327255588E-16,-0.998698786790945));
#15440=DIRECTION('center_axis',(1.,0.,0.));
#15441=DIRECTION('ref_axis',(0.,0.,1.));
#15442=DIRECTION('center_axis',(-1.,0.,0.));
#15443=DIRECTION('ref_axis',(0.,0.,-1.));
#15444=DIRECTION('center_axis',(1.,0.,0.));
#15445=DIRECTION('ref_axis',(0.,0.,1.));
#15446=DIRECTION('',(-0.0509973848574056,1.22305327255588E-16,0.998698786790945));
#15447=DIRECTION('center_axis',(1.,0.,0.));
#15448=DIRECTION('ref_axis',(0.,0.,1.));
#15449=DIRECTION('center_axis',(1.,0.,0.));
#15450=DIRECTION('ref_axis',(0.,0.,1.));
#15451=DIRECTION('center_axis',(-1.,0.,0.));
#15452=DIRECTION('ref_axis',(0.,0.,-1.));
#15453=DIRECTION('center_axis',(1.,0.,0.));
#15454=DIRECTION('ref_axis',(0.,0.,1.));
#15455=DIRECTION('',(0.101599191217213,-1.21830975896784E-16,-0.994825414001878));
#15456=DIRECTION('center_axis',(1.,0.,0.));
#15457=DIRECTION('ref_axis',(0.,0.,1.));
#15458=DIRECTION('center_axis',(1.,0.,0.));
#15459=DIRECTION('ref_axis',(0.,0.,1.));
#15460=DIRECTION('center_axis',(1.,0.,0.));
#15461=DIRECTION('ref_axis',(0.,0.,1.));
#15462=DIRECTION('center_axis',(1.,0.,0.));
#15463=DIRECTION('ref_axis',(0.,0.,1.));
#15464=DIRECTION('',(0.0509973848574056,1.22305327255588E-16,-0.998698786790945));
#15465=DIRECTION('center_axis',(1.,0.,0.));
#15466=DIRECTION('ref_axis',(0.,0.,1.));
#15467=DIRECTION('center_axis',(1.,0.,0.));
#15468=DIRECTION('ref_axis',(0.,0.,1.));
#15469=DIRECTION('center_axis',(1.,0.,0.));
#15470=DIRECTION('ref_axis',(0.,0.,1.));
#15471=DIRECTION('center_axis',(1.,0.,0.));
#15472=DIRECTION('ref_axis',(0.,0.,1.));
#15473=DIRECTION('',(-0.0509973848574156,-1.22305327255588E-16,0.998698786790945));
#15474=DIRECTION('center_axis',(1.,0.,0.));
#15475=DIRECTION('ref_axis',(0.,0.,1.));
#15476=DIRECTION('center_axis',(-1.,0.,0.));
#15477=DIRECTION('ref_axis',(0.,0.,-1.));
#15478=DIRECTION('',(-0.0509973848574156,1.22305327255587E-16,0.998698786790945));
#15479=DIRECTION('center_axis',(1.,0.,0.));
#15480=DIRECTION('ref_axis',(0.,0.,1.));
#15481=DIRECTION('center_axis',(1.,0.,0.));
#15482=DIRECTION('ref_axis',(0.,0.,1.));
#15483=DIRECTION('center_axis',(1.,0.,0.));
#15484=DIRECTION('ref_axis',(0.,0.,1.));
#15485=DIRECTION('',(-1.,0.,0.));
#15486=DIRECTION('center_axis',(1.,0.,0.));
#15487=DIRECTION('ref_axis',(0.,0.,1.));
#15488=DIRECTION('',(-1.,0.,0.));
#15489=DIRECTION('center_axis',(1.,0.,0.));
#15490=DIRECTION('ref_axis',(0.,0.,1.));
#15491=DIRECTION('center_axis',(1.,0.,0.));
#15492=DIRECTION('ref_axis',(0.,0.,1.));
#15493=DIRECTION('',(-1.,0.,0.));
#15494=DIRECTION('center_axis',(1.,0.,0.));
#15495=DIRECTION('ref_axis',(0.,0.,1.));
#15496=DIRECTION('center_axis',(1.,0.,0.));
#15497=DIRECTION('ref_axis',(0.,0.,1.));
#15498=DIRECTION('center_axis',(1.,0.,0.));
#15499=DIRECTION('ref_axis',(0.,0.,1.));
#15500=DIRECTION('center_axis',(0.,1.,1.22464679914735E-16));
#15501=DIRECTION('ref_axis',(0.,1.22464679914735E-16,-1.));
#15502=DIRECTION('center_axis',(1.,0.,0.));
#15503=DIRECTION('ref_axis',(0.,0.,1.));
#15504=DIRECTION('center_axis',(1.,0.,0.));
#15505=DIRECTION('ref_axis',(0.,0.,1.));
#15506=DIRECTION('center_axis',(0.,1.,1.22464679914735E-16));
#15507=DIRECTION('ref_axis',(0.,1.22464679914735E-16,-1.));
#15508=DIRECTION('center_axis',(1.,0.,0.));
#15509=DIRECTION('ref_axis',(0.,0.,1.));
#15510=DIRECTION('center_axis',(1.,0.,0.));
#15511=DIRECTION('ref_axis',(0.,0.,1.));
#15512=DIRECTION('center_axis',(1.,0.,0.));
#15513=DIRECTION('ref_axis',(0.,0.,1.));
#15514=DIRECTION('',(1.,0.,0.));
#15515=DIRECTION('center_axis',(1.,0.,0.));
#15516=DIRECTION('ref_axis',(0.,0.,1.));
#15517=DIRECTION('center_axis',(1.,0.,0.));
#15518=DIRECTION('ref_axis',(0.,0.,1.));
#15519=DIRECTION('center_axis',(0.,1.,1.22464679914735E-16));
#15520=DIRECTION('ref_axis',(0.,1.22464679914735E-16,-1.));
#15521=DIRECTION('center_axis',(1.,0.,0.));
#15522=DIRECTION('ref_axis',(0.,0.,1.));
#15523=DIRECTION('center_axis',(1.,0.,0.));
#15524=DIRECTION('ref_axis',(0.,0.,1.));
#15525=DIRECTION('center_axis',(0.,1.,1.22464679914735E-16));
#15526=DIRECTION('ref_axis',(0.,1.22464679914735E-16,-1.));
#15527=DIRECTION('center_axis',(1.,0.,0.));
#15528=DIRECTION('ref_axis',(0.,0.,1.));
#15529=DIRECTION('center_axis',(1.,0.,0.));
#15530=DIRECTION('ref_axis',(0.,0.,1.));
#15531=DIRECTION('center_axis',(1.,0.,0.));
#15532=DIRECTION('ref_axis',(0.,0.,1.));
#15533=DIRECTION('',(-1.,0.,0.));
#15534=DIRECTION('center_axis',(1.,0.,0.));
#15535=DIRECTION('ref_axis',(0.,0.,1.));
#15536=DIRECTION('',(-1.,0.,0.));
#15537=DIRECTION('center_axis',(-1.,0.,0.));
#15538=DIRECTION('ref_axis',(0.,0.,-1.));
#15539=DIRECTION('center_axis',(1.,0.,0.));
#15540=DIRECTION('ref_axis',(0.,-1.,0.));
#15541=DIRECTION('center_axis',(-1.,0.,0.));
#15542=DIRECTION('ref_axis',(0.,0.,-1.));
#15543=DIRECTION('center_axis',(1.,0.,0.));
#15544=DIRECTION('ref_axis',(0.,-1.,0.));
#15545=DIRECTION('center_axis',(-1.,0.,0.));
#15546=DIRECTION('ref_axis',(0.,0.,-1.));
#15547=DIRECTION('center_axis',(1.,0.,0.));
#15548=DIRECTION('ref_axis',(0.,-1.,0.));
#15549=DIRECTION('',(1.,-7.70371977754894E-34,0.));
#15550=DIRECTION('',(-6.41463530422127E-50,-8.32667268468868E-17,-1.));
#15551=DIRECTION('',(0.,0.,1.));
#15552=DIRECTION('',(1.,0.,0.));
#15553=DIRECTION('',(0.,0.,1.));
#15554=DIRECTION('',(1.,0.,0.));
#15555=DIRECTION('',(6.93889390390722E-17,1.55431223447522E-15,-1.));
#15556=DIRECTION('',(-1.,-1.11022302462516E-16,-6.93889390390724E-17));
#15557=DIRECTION('',(5.72458747072346E-17,1.77635683940025E-15,-1.));
#15558=DIRECTION('',(-1.,6.93889390390726E-18,-5.72458747072346E-17));
#15559=DIRECTION('',(1.,-3.17567743784134E-16,-3.05311331771918E-16));
#15560=DIRECTION('',(-3.05311331771918E-16,2.16936748935778E-30,-1.));
#15561=DIRECTION('',(0.,0.,-1.));
#15562=DIRECTION('',(-1.,2.77555756156289E-16,0.));
#15563=DIRECTION('',(0.,0.,1.));
#15564=DIRECTION('',(1.,0.,0.));
#15565=DIRECTION('',(0.,0.,1.));
#15566=DIRECTION('',(1.,0.,0.));
#15567=DIRECTION('',(-1.29592398829528E-15,1.,0.));
#15568=DIRECTION('',(0.,0.,1.));
#15569=DIRECTION('',(1.,0.,0.));
#15570=DIRECTION('',(0.,0.,-1.));
#15571=DIRECTION('',(0.,0.,1.));
#15572=DIRECTION('',(0.921006233605332,-0.389547837447625,0.));
#15573=DIRECTION('',(0.,0.,-1.));
#15574=DIRECTION('',(1.,-1.73472347597681E-17,0.));
#15575=DIRECTION('',(0.,0.,1.));
#15576=DIRECTION('',(0.770032315674686,0.638004884633872,0.));
#15577=DIRECTION('',(1.,0.,0.));
#15578=DIRECTION('',(0.,0.,-1.));
#15579=DIRECTION('',(0.,0.,1.));
#15580=DIRECTION('',(1.,0.,0.));
#15581=DIRECTION('',(1.,0.,0.));
#15582=DIRECTION('',(0.,-1.54683223344484E-16,-1.));
#15583=DIRECTION('',(1.,-3.17567743784134E-16,-3.05311331771918E-16));
#15584=DIRECTION('',(-3.05311331771918E-16,2.16936748935778E-30,-1.));
#15585=DIRECTION('',(0.,0.,1.));
#15586=DIRECTION('',(1.,0.,0.));
#15587=DIRECTION('',(0.,0.,1.));
#15588=DIRECTION('',(1.,0.,0.));
#15589=DIRECTION('',(0.,0.,-1.));
#15590=DIRECTION('',(-1.,2.77555756156289E-16,0.));
#15591=DIRECTION('',(0.,0.,1.));
#15592=DIRECTION('',(1.,0.,0.));
#15593=DIRECTION('',(2.77555756156289E-17,-6.16297582203915E-33,-1.));
#15594=DIRECTION('',(-1.,-1.66533453693773E-16,-2.77555756156289E-17));
#15595=DIRECTION('',(2.77555756156289E-17,-6.16297582203915E-33,-1.));
#15596=DIRECTION('',(-1.,-1.66533453693773E-16,-2.77555756156289E-17));
#15597=DIRECTION('',(0.,0.,1.));
#15598=DIRECTION('',(1.,0.,0.));
#15599=DIRECTION('',(-1.,0.,0.));
#15600=DIRECTION('',(0.,0.,1.));
#15601=DIRECTION('',(-1.,1.55431223447522E-15,-6.93889390390698E-17));
#15602=DIRECTION('',(-6.93889390390722E-17,-1.55431223447522E-15,1.));
#15603=DIRECTION('',(1.,1.77635683940025E-15,5.72458747072378E-17));
#15604=DIRECTION('',(5.72458747072346E-17,1.77635683940025E-15,-1.));
#15605=CARTESIAN_POINT('',(0.,0.,0.));
#15606=CARTESIAN_POINT('',(0.,0.,0.));
#15607=CARTESIAN_POINT('Origin',(198.2,9.50000000000001,9.));
#15608=CARTESIAN_POINT('',(200.2,9.50000000000001,9.));
#15609=CARTESIAN_POINT('Origin',(198.2,9.50000000000001,9.));
#15610=CARTESIAN_POINT('',(200.2,9.50000000000001,3.));
#15611=CARTESIAN_POINT('',(200.2,9.50000000000001,9.));
#15612=CARTESIAN_POINT('Origin',(198.2,9.50000000000001,3.));
#15613=CARTESIAN_POINT('Origin',(198.2,-4.49999999999994,9.));
#15614=CARTESIAN_POINT('',(200.2,-4.49999999999994,9.));
#15615=CARTESIAN_POINT('Origin',(198.2,-4.49999999999994,9.));
#15616=CARTESIAN_POINT('',(200.2,-4.49999999999994,3.));
#15617=CARTESIAN_POINT('',(200.2,-4.49999999999994,9.));
#15618=CARTESIAN_POINT('Origin',(198.2,-4.49999999999994,3.));
#15619=CARTESIAN_POINT('Origin',(162.5,0.,9.));
#15620=CARTESIAN_POINT('',(158.5,-4.89858719658942E-16,4.6));
#15621=CARTESIAN_POINT('Origin',(162.5,0.,4.6));
#15622=CARTESIAN_POINT('',(158.5,-4.89858719658942E-16,9.));
#15623=CARTESIAN_POINT('',(158.5,-4.89858719658942E-16,9.));
#15624=CARTESIAN_POINT('Origin',(162.5,0.,9.));
#15625=CARTESIAN_POINT('Origin',(162.5,0.,9.));
#15626=CARTESIAN_POINT('',(160.25,-2.75545529808155E-16,1.));
#15627=CARTESIAN_POINT('Origin',(162.5,-2.31296463463574E-16,1.));
#15628=CARTESIAN_POINT('',(160.25,-2.75545529808155E-16,4.6));
#15629=CARTESIAN_POINT('',(160.25,-2.75545529808155E-16,9.));
#15630=CARTESIAN_POINT('Origin',(162.5,0.,4.6));
#15631=CARTESIAN_POINT('Origin',(182.5,0.,9.));
#15632=CARTESIAN_POINT('',(178.5,-4.89858719658942E-16,4.6));
#15633=CARTESIAN_POINT('Origin',(182.5,0.,4.6));
#15634=CARTESIAN_POINT('',(178.5,-4.89858719658942E-16,9.));
#15635=CARTESIAN_POINT('',(178.5,-4.89858719658942E-16,9.));
#15636=CARTESIAN_POINT('Origin',(182.5,0.,9.));
#15637=CARTESIAN_POINT('Origin',(182.5,0.,9.));
#15638=CARTESIAN_POINT('',(180.25,-2.75545529808155E-16,1.));
#15639=CARTESIAN_POINT('Origin',(182.5,-2.31296463463574E-16,1.));
#15640=CARTESIAN_POINT('',(180.25,-2.75545529808155E-16,4.6));
#15641=CARTESIAN_POINT('',(180.25,-2.75545529808155E-16,9.));
#15642=CARTESIAN_POINT('Origin',(182.5,0.,4.6));
#15643=CARTESIAN_POINT('Origin',(212.,2.50000000000003,9.));
#15644=CARTESIAN_POINT('',(219.,2.50000000000003,9.));
#15645=CARTESIAN_POINT('Origin',(212.,2.50000000000003,9.));
#15646=CARTESIAN_POINT('',(219.,2.50000000000003,8.));
#15647=CARTESIAN_POINT('',(219.,2.50000000000003,9.));
#15648=CARTESIAN_POINT('Origin',(212.,2.50000000000003,8.));
#15649=CARTESIAN_POINT('Origin',(212.,2.50000000000003,8.));
#15650=CARTESIAN_POINT('',(222.,2.50000000000003,8.));
#15651=CARTESIAN_POINT('Origin',(212.,2.50000000000003,8.));
#15652=CARTESIAN_POINT('',(222.,2.50000000000003,7.));
#15653=CARTESIAN_POINT('',(222.,2.50000000000003,8.));
#15654=CARTESIAN_POINT('Origin',(212.,2.50000000000003,7.));
#15655=CARTESIAN_POINT('Origin',(212.,2.50000000000003,7.));
#15656=CARTESIAN_POINT('',(223.1,2.50000000000003,7.));
#15657=CARTESIAN_POINT('Origin',(212.,2.50000000000003,7.));
#15658=CARTESIAN_POINT('',(223.1,2.50000000000003,0.));
#15659=CARTESIAN_POINT('',(223.1,2.50000000000003,7.));
#15660=CARTESIAN_POINT('Origin',(212.,2.50000000000003,0.));
#15661=CARTESIAN_POINT('Origin',(190.,0.,-10.));
#15662=CARTESIAN_POINT('',(190.,-3.95,1.));
#15663=CARTESIAN_POINT('',(190.,-3.95,3.));
#15664=CARTESIAN_POINT('',(190.,-3.95,1.));
#15665=CARTESIAN_POINT('',(190.,3.95,1.));
#15666=CARTESIAN_POINT('',(190.,-3.95,1.));
#15667=CARTESIAN_POINT('',(190.,3.95,3.));
#15668=CARTESIAN_POINT('',(190.,3.95,1.));
#15669=CARTESIAN_POINT('',(190.,15.,3.));
#15670=CARTESIAN_POINT('',(190.,15.,3.));
#15671=CARTESIAN_POINT('',(190.,15.,-10.));
#15672=CARTESIAN_POINT('',(190.,15.,3.));
#15673=CARTESIAN_POINT('',(190.,-13.9772819352292,-10.));
#15674=CARTESIAN_POINT('',(190.,0.,-10.));
#15675=CARTESIAN_POINT('',(190.,-13.9772819352292,0.));
#15676=CARTESIAN_POINT('',(190.,-13.9772819352292,-10.));
#15677=CARTESIAN_POINT('',(190.,-15.,0.));
#15678=CARTESIAN_POINT('',(190.,0.,0.));
#15679=CARTESIAN_POINT('',(190.,-15.,3.));
#15680=CARTESIAN_POINT('',(190.,-15.,3.));
#15681=CARTESIAN_POINT('',(190.,15.,3.));
#15682=CARTESIAN_POINT('Origin',(190.,15.,3.));
#15683=CARTESIAN_POINT('',(155.,-3.94999999999999,3.));
#15684=CARTESIAN_POINT('',(155.,-3.95,3.));
#15685=CARTESIAN_POINT('',(157.,-15.,3.));
#15686=CARTESIAN_POINT('',(190.,-15.,3.));
#15687=CARTESIAN_POINT('',(155.,-13.,3.));
#15688=CARTESIAN_POINT('Origin',(157.,-13.,3.));
#15689=CARTESIAN_POINT('',(155.,15.,3.));
#15690=CARTESIAN_POINT('Origin',(190.,15.,3.));
#15691=CARTESIAN_POINT('',(155.,3.95,3.));
#15692=CARTESIAN_POINT('',(155.,3.95,3.));
#15693=CARTESIAN_POINT('',(155.,13.,3.));
#15694=CARTESIAN_POINT('',(155.,15.,3.));
#15695=CARTESIAN_POINT('',(157.,15.,3.));
#15696=CARTESIAN_POINT('Origin',(157.,13.,3.));
#15697=CARTESIAN_POINT('',(190.,15.,3.));
#15698=CARTESIAN_POINT('Origin',(0.,0.,0.));
#15699=CARTESIAN_POINT('',(195.,13.,0.));
#15700=CARTESIAN_POINT('',(203.5,13.,0.));
#15701=CARTESIAN_POINT('',(190.,13.,0.));
#15702=CARTESIAN_POINT('',(205.,13.8660254037845,0.));
#15703=CARTESIAN_POINT('',(45.2458348754007,-78.3680848350663,0.));
#15704=CARTESIAN_POINT('',(205.,15.,0.));
#15705=CARTESIAN_POINT('',(205.,13.,0.));
#15706=CARTESIAN_POINT('',(212.,15.,0.));
#15707=CARTESIAN_POINT('',(0.,15.,0.));
#15708=CARTESIAN_POINT('',(214.620037028164,-9.72233226397694,0.));
#15709=CARTESIAN_POINT('Origin',(212.,2.50000000000003,0.));
#15710=CARTESIAN_POINT('',(11.4215507970056,-53.2809221054195,0.));
#15711=CARTESIAN_POINT('',(195.,-12.9054582556007,0.));
#15712=CARTESIAN_POINT('',(11.2119478347524,-52.3031355243012,0.));
#15713=CARTESIAN_POINT('',(195.,0.,0.));
#15714=CARTESIAN_POINT('',(201.2,11.2320508075689,0.));
#15715=CARTESIAN_POINT('',(201.2,7.76794919243114,0.));
#15716=CARTESIAN_POINT('',(201.2,11.2320508075689,0.));
#15717=CARTESIAN_POINT('',(198.2,12.9641016151378,0.));
#15718=CARTESIAN_POINT('',(198.2,12.9641016151378,0.));
#15719=CARTESIAN_POINT('',(195.2,11.2320508075689,0.));
#15720=CARTESIAN_POINT('',(195.2,11.2320508075689,0.));
#15721=CARTESIAN_POINT('',(195.2,7.76794919243112,0.));
#15722=CARTESIAN_POINT('',(195.2,7.76794919243112,0.));
#15723=CARTESIAN_POINT('',(198.2,6.03589838486225,0.));
#15724=CARTESIAN_POINT('',(198.2,6.03589838486225,0.));
#15725=CARTESIAN_POINT('',(201.2,7.76794919243114,0.));
#15726=CARTESIAN_POINT('',(195.2,-6.23205080756882,0.));
#15727=CARTESIAN_POINT('',(195.2,-2.76794919243105,0.));
#15728=CARTESIAN_POINT('',(195.2,-2.76794919243105,0.));
#15729=CARTESIAN_POINT('',(198.2,-7.9641016151377,0.));
#15730=CARTESIAN_POINT('',(195.2,-6.23205080756882,0.));
#15731=CARTESIAN_POINT('',(201.2,-6.23205080756883,0.));
#15732=CARTESIAN_POINT('',(198.2,-7.9641016151377,0.));
#15733=CARTESIAN_POINT('',(201.2,-2.76794919243107,0.));
#15734=CARTESIAN_POINT('',(201.2,-6.23205080756883,0.));
#15735=CARTESIAN_POINT('',(198.2,-1.03589838486218,0.));
#15736=CARTESIAN_POINT('',(201.2,-2.76794919243107,0.));
#15737=CARTESIAN_POINT('',(198.2,-1.03589838486218,0.));
#15738=CARTESIAN_POINT('Origin',(11.4215507970056,-53.2809221054195,9.));
#15739=CARTESIAN_POINT('',(214.620037028164,-9.72233226397694,9.));
#15740=CARTESIAN_POINT('',(214.620037028164,-9.72233226397694,9.));
#15741=CARTESIAN_POINT('',(190.,-15.,9.));
#15742=CARTESIAN_POINT('',(11.4215507970056,-53.2809221054195,9.));
#15743=CARTESIAN_POINT('',(190.,-15.,9.));
#15744=CARTESIAN_POINT('Origin',(212.,2.50000000000003,9.));
#15745=CARTESIAN_POINT('',(212.,15.,9.));
#15746=CARTESIAN_POINT('',(212.,15.,9.));
#15747=CARTESIAN_POINT('Origin',(212.,2.50000000000003,9.));
#15748=CARTESIAN_POINT('Origin',(0.,15.,9.));
#15749=CARTESIAN_POINT('',(157.,15.,9.));
#15750=CARTESIAN_POINT('',(157.,15.,9.));
#15751=CARTESIAN_POINT('',(0.,15.,9.));
#15752=CARTESIAN_POINT('',(205.,15.,-10.));
#15753=CARTESIAN_POINT('',(205.,15.,0.));
#15754=CARTESIAN_POINT('',(190.,15.,-10.));
#15755=CARTESIAN_POINT('Origin',(155.,0.,9.));
#15756=CARTESIAN_POINT('',(155.,13.,9.));
#15757=CARTESIAN_POINT('',(155.,13.,0.));
#15758=CARTESIAN_POINT('',(155.,3.95,1.));
#15759=CARTESIAN_POINT('',(155.,3.95,1.));
#15760=CARTESIAN_POINT('',(155.,-3.95,1.));
#15761=CARTESIAN_POINT('',(155.,-3.95,1.));
#15762=CARTESIAN_POINT('',(155.,-3.95,1.));
#15763=CARTESIAN_POINT('',(155.,-13.,9.));
#15764=CARTESIAN_POINT('',(155.,-13.,9.));
#15765=CARTESIAN_POINT('',(155.,0.,9.));
#15766=CARTESIAN_POINT('Origin',(1.48690583655155E-15,-15.,9.));
#15767=CARTESIAN_POINT('',(157.,-15.,9.));
#15768=CARTESIAN_POINT('',(157.,-15.,9.));
#15769=CARTESIAN_POINT('',(1.48690583655155E-15,-15.,9.));
#15770=CARTESIAN_POINT('Origin',(0.,0.,9.));
#15771=CARTESIAN_POINT('Origin',(157.,-13.,9.));
#15772=CARTESIAN_POINT('Origin',(157.,13.,9.));
#15773=CARTESIAN_POINT('Origin',(212.,2.50000000000003,7.));
#15774=CARTESIAN_POINT('Origin',(212.,2.50000000000003,8.));
#15775=CARTESIAN_POINT('Origin',(11.2119478347524,-52.3031355243012,-10.));
#15776=CARTESIAN_POINT('',(195.,-12.9054582556007,-10.));
#15777=CARTESIAN_POINT('',(11.2119478347524,-52.3031355243012,-10.));
#15778=CARTESIAN_POINT('',(195.,-12.9054582556007,-10.));
#15779=CARTESIAN_POINT('Origin',(195.,0.,-10.));
#15780=CARTESIAN_POINT('',(195.,13.,-10.));
#15781=CARTESIAN_POINT('',(195.,0.,-10.));
#15782=CARTESIAN_POINT('',(195.,13.,-10.));
#15783=CARTESIAN_POINT('Origin',(0.,0.,-10.));
#15784=CARTESIAN_POINT('',(205.,13.8660254037845,-10.));
#15785=CARTESIAN_POINT('',(205.,13.,-10.));
#15786=CARTESIAN_POINT('',(203.5,13.,-10.));
#15787=CARTESIAN_POINT('',(45.2458348754007,-78.3680848350663,-10.));
#15788=CARTESIAN_POINT('',(190.,13.,-10.));
#15789=CARTESIAN_POINT('Origin',(157.,-13.,9.));
#15790=CARTESIAN_POINT('Origin',(157.,13.,9.));
#15791=CARTESIAN_POINT('Origin',(184.75,0.,4.6));
#15792=CARTESIAN_POINT('Origin',(164.75,0.,4.6));
#15793=CARTESIAN_POINT('Origin',(195.2,-6.23205080756882,3.));
#15794=CARTESIAN_POINT('',(195.2,-6.23205080756882,3.));
#15795=CARTESIAN_POINT('',(195.2,-6.23205080756882,3.));
#15796=CARTESIAN_POINT('',(198.2,-7.9641016151377,3.));
#15797=CARTESIAN_POINT('',(195.2,-6.23205080756882,3.));
#15798=CARTESIAN_POINT('',(198.2,-7.9641016151377,3.));
#15799=CARTESIAN_POINT('Origin',(198.2,-7.9641016151377,3.));
#15800=CARTESIAN_POINT('',(201.2,-6.23205080756883,3.));
#15801=CARTESIAN_POINT('',(198.2,-7.9641016151377,3.));
#15802=CARTESIAN_POINT('',(201.2,-6.23205080756883,3.));
#15803=CARTESIAN_POINT('Origin',(201.2,-6.23205080756883,3.));
#15804=CARTESIAN_POINT('',(201.2,-2.76794919243107,3.));
#15805=CARTESIAN_POINT('',(201.2,-6.23205080756883,3.));
#15806=CARTESIAN_POINT('',(201.2,-2.76794919243107,3.));
#15807=CARTESIAN_POINT('Origin',(201.2,-2.76794919243107,3.));
#15808=CARTESIAN_POINT('',(198.2,-1.03589838486218,3.));
#15809=CARTESIAN_POINT('',(201.2,-2.76794919243107,3.));
#15810=CARTESIAN_POINT('',(198.2,-1.03589838486218,3.));
#15811=CARTESIAN_POINT('Origin',(198.2,-1.03589838486218,3.));
#15812=CARTESIAN_POINT('',(195.2,-2.76794919243105,3.));
#15813=CARTESIAN_POINT('',(198.2,-1.03589838486218,3.));
#15814=CARTESIAN_POINT('',(195.2,-2.76794919243105,3.));
#15815=CARTESIAN_POINT('Origin',(195.2,-2.76794919243105,3.));
#15816=CARTESIAN_POINT('',(195.2,-2.76794919243105,3.));
#15817=CARTESIAN_POINT('Origin',(0.,0.,3.));
#15818=CARTESIAN_POINT('Origin',(198.2,12.9641016151378,3.));
#15819=CARTESIAN_POINT('',(201.2,11.2320508075689,3.));
#15820=CARTESIAN_POINT('',(201.2,11.2320508075689,3.));
#15821=CARTESIAN_POINT('',(198.2,12.9641016151378,3.));
#15822=CARTESIAN_POINT('',(198.2,12.9641016151378,3.));
#15823=CARTESIAN_POINT('',(198.2,12.9641016151378,3.));
#15824=CARTESIAN_POINT('Origin',(195.2,11.2320508075689,3.));
#15825=CARTESIAN_POINT('',(195.2,11.2320508075689,3.));
#15826=CARTESIAN_POINT('',(195.2,11.2320508075689,3.));
#15827=CARTESIAN_POINT('',(195.2,11.2320508075689,3.));
#15828=CARTESIAN_POINT('Origin',(195.2,7.76794919243112,3.));
#15829=CARTESIAN_POINT('',(195.2,7.76794919243112,3.));
#15830=CARTESIAN_POINT('',(195.2,7.76794919243112,3.));
#15831=CARTESIAN_POINT('',(195.2,7.76794919243112,3.));
#15832=CARTESIAN_POINT('Origin',(198.2,6.03589838486225,3.));
#15833=CARTESIAN_POINT('',(198.2,6.03589838486225,3.));
#15834=CARTESIAN_POINT('',(198.2,6.03589838486225,3.));
#15835=CARTESIAN_POINT('',(198.2,6.03589838486225,3.));
#15836=CARTESIAN_POINT('Origin',(201.2,7.76794919243114,3.));
#15837=CARTESIAN_POINT('',(201.2,7.76794919243114,3.));
#15838=CARTESIAN_POINT('',(201.2,7.76794919243114,3.));
#15839=CARTESIAN_POINT('',(201.2,7.76794919243114,3.));
#15840=CARTESIAN_POINT('Origin',(201.2,11.2320508075689,3.));
#15841=CARTESIAN_POINT('',(201.2,11.2320508075689,3.));
#15842=CARTESIAN_POINT('Origin',(0.,0.,3.));
#15843=CARTESIAN_POINT('Origin',(0.,13.,0.));
#15844=CARTESIAN_POINT('',(203.5,13.,0.));
#15845=CARTESIAN_POINT('Origin',(205.,13.,0.));
#15846=CARTESIAN_POINT('',(205.,13.8660254037845,0.));
#15847=CARTESIAN_POINT('Origin',(205.,13.8660254037845,0.));
#15848=CARTESIAN_POINT('Origin',(0.,9.80814117218957E-17,1.));
#15849=CARTESIAN_POINT('',(155.,-3.95,1.));
#15850=CARTESIAN_POINT('',(155.,3.95,1.));
#15851=CARTESIAN_POINT('Origin',(155.,-3.95,1.));
#15852=CARTESIAN_POINT('Origin',(155.,3.95,1.));
#15853=CARTESIAN_POINT('',(0.,0.,0.));
#15854=CARTESIAN_POINT('Origin',(198.2,9.50000000000001,-9.));
#15855=CARTESIAN_POINT('',(200.2,9.50000000000001,-9.));
#15856=CARTESIAN_POINT('Origin',(198.2,9.50000000000001,-9.));
#15857=CARTESIAN_POINT('',(200.2,9.50000000000001,-3.));
#15858=CARTESIAN_POINT('',(200.2,9.50000000000001,-9.));
#15859=CARTESIAN_POINT('Origin',(198.2,9.50000000000001,-3.));
#15860=CARTESIAN_POINT('Origin',(198.2,-4.49999999999994,-9.));
#15861=CARTESIAN_POINT('',(200.2,-4.49999999999994,-9.));
#15862=CARTESIAN_POINT('Origin',(198.2,-4.49999999999994,-9.));
#15863=CARTESIAN_POINT('',(200.2,-4.49999999999994,-3.));
#15864=CARTESIAN_POINT('',(200.2,-4.49999999999994,-9.));
#15865=CARTESIAN_POINT('Origin',(198.2,-4.49999999999994,-3.));
#15866=CARTESIAN_POINT('Origin',(162.5,0.,-9.));
#15867=CARTESIAN_POINT('',(158.5,4.89858719658942E-16,-4.6));
#15868=CARTESIAN_POINT('Origin',(162.5,0.,-4.6));
#15869=CARTESIAN_POINT('',(158.5,4.89858719658942E-16,-9.));
#15870=CARTESIAN_POINT('',(158.5,4.89858719658942E-16,-9.));
#15871=CARTESIAN_POINT('Origin',(162.5,0.,-9.));
#15872=CARTESIAN_POINT('Origin',(162.5,0.,-9.));
#15873=CARTESIAN_POINT('',(160.25,2.75545529808155E-16,-1.));
#15874=CARTESIAN_POINT('Origin',(162.5,-2.31296463463574E-16,-1.));
#15875=CARTESIAN_POINT('',(160.25,2.75545529808155E-16,-4.6));
#15876=CARTESIAN_POINT('',(160.25,2.75545529808155E-16,-9.));
#15877=CARTESIAN_POINT('Origin',(162.5,0.,-4.6));
#15878=CARTESIAN_POINT('Origin',(182.5,0.,-9.));
#15879=CARTESIAN_POINT('',(178.5,4.89858719658942E-16,-4.6));
#15880=CARTESIAN_POINT('Origin',(182.5,0.,-4.6));
#15881=CARTESIAN_POINT('',(178.5,4.89858719658942E-16,-9.));
#15882=CARTESIAN_POINT('',(178.5,4.89858719658942E-16,-9.));
#15883=CARTESIAN_POINT('Origin',(182.5,0.,-9.));
#15884=CARTESIAN_POINT('Origin',(182.5,0.,-9.));
#15885=CARTESIAN_POINT('',(180.25,2.75545529808155E-16,-1.));
#15886=CARTESIAN_POINT('Origin',(182.5,-2.31296463463574E-16,-1.));
#15887=CARTESIAN_POINT('',(180.25,2.75545529808155E-16,-4.6));
#15888=CARTESIAN_POINT('',(180.25,2.75545529808155E-16,-9.));
#15889=CARTESIAN_POINT('Origin',(182.5,0.,-4.6));
#15890=CARTESIAN_POINT('Origin',(212.,2.50000000000003,-9.));
#15891=CARTESIAN_POINT('',(219.,2.50000000000003,-9.));
#15892=CARTESIAN_POINT('Origin',(212.,2.50000000000003,-9.));
#15893=CARTESIAN_POINT('',(219.,2.50000000000003,-8.));
#15894=CARTESIAN_POINT('',(219.,2.50000000000003,-9.));
#15895=CARTESIAN_POINT('Origin',(212.,2.50000000000003,-8.));
#15896=CARTESIAN_POINT('Origin',(212.,2.50000000000003,-8.));
#15897=CARTESIAN_POINT('',(222.,2.50000000000003,-8.));
#15898=CARTESIAN_POINT('Origin',(212.,2.50000000000003,-8.));
#15899=CARTESIAN_POINT('',(222.,2.50000000000003,-7.));
#15900=CARTESIAN_POINT('',(222.,2.50000000000003,-8.));
#15901=CARTESIAN_POINT('Origin',(212.,2.50000000000003,-7.));
#15902=CARTESIAN_POINT('Origin',(212.,2.50000000000003,-7.));
#15903=CARTESIAN_POINT('',(223.1,2.50000000000003,-7.));
#15904=CARTESIAN_POINT('Origin',(212.,2.50000000000003,-7.));
#15905=CARTESIAN_POINT('',(223.1,2.50000000000003,0.));
#15906=CARTESIAN_POINT('',(223.1,2.50000000000003,-7.));
#15907=CARTESIAN_POINT('Origin',(212.,2.50000000000003,0.));
#15908=CARTESIAN_POINT('Origin',(190.,0.,10.));
#15909=CARTESIAN_POINT('',(190.,-3.95,-1.));
#15910=CARTESIAN_POINT('',(190.,-3.95,-3.));
#15911=CARTESIAN_POINT('',(190.,-3.95,-1.));
#15912=CARTESIAN_POINT('',(190.,-15.,-3.));
#15913=CARTESIAN_POINT('',(190.,15.,-3.));
#15914=CARTESIAN_POINT('',(190.,-15.,0.));
#15915=CARTESIAN_POINT('',(190.,-15.,-3.));
#15916=CARTESIAN_POINT('',(190.,-13.9772819352292,0.));
#15917=CARTESIAN_POINT('',(190.,0.,0.));
#15918=CARTESIAN_POINT('',(190.,-13.9772819352292,10.));
#15919=CARTESIAN_POINT('',(190.,-13.9772819352292,10.));
#15920=CARTESIAN_POINT('',(190.,15.,10.));
#15921=CARTESIAN_POINT('',(190.,0.,10.));
#15922=CARTESIAN_POINT('',(190.,15.,-3.));
#15923=CARTESIAN_POINT('',(190.,15.,-3.));
#15924=CARTESIAN_POINT('',(190.,3.95,-3.));
#15925=CARTESIAN_POINT('',(190.,15.,-3.));
#15926=CARTESIAN_POINT('',(190.,3.95,-1.));
#15927=CARTESIAN_POINT('',(190.,3.95,-1.));
#15928=CARTESIAN_POINT('',(190.,-3.95,-1.));
#15929=CARTESIAN_POINT('Origin',(190.,15.,-3.));
#15930=CARTESIAN_POINT('',(155.,-3.94999999999999,-3.));
#15931=CARTESIAN_POINT('',(155.,-3.95,-3.));
#15932=CARTESIAN_POINT('',(155.,-13.,-3.));
#15933=CARTESIAN_POINT('',(155.,15.,-3.));
#15934=CARTESIAN_POINT('',(157.,-15.,-3.));
#15935=CARTESIAN_POINT('Origin',(157.,-13.,-3.));
#15936=CARTESIAN_POINT('',(190.,-15.,-3.));
#15937=CARTESIAN_POINT('Origin',(190.,15.,-3.));
#15938=CARTESIAN_POINT('',(155.,3.95,-3.));
#15939=CARTESIAN_POINT('',(155.,3.95,-3.));
#15940=CARTESIAN_POINT('',(157.,15.,-3.));
#15941=CARTESIAN_POINT('',(190.,15.,-3.));
#15942=CARTESIAN_POINT('',(155.,13.,-3.));
#15943=CARTESIAN_POINT('Origin',(157.,13.,-3.));
#15944=CARTESIAN_POINT('',(155.,15.,-3.));
#15945=CARTESIAN_POINT('Origin',(0.,0.,0.));
#15946=CARTESIAN_POINT('',(195.,13.,0.));
#15947=CARTESIAN_POINT('',(203.5,13.,0.));
#15948=CARTESIAN_POINT('',(190.,13.,0.));
#15949=CARTESIAN_POINT('',(195.,-12.9054582556007,0.));
#15950=CARTESIAN_POINT('',(195.,0.,0.));
#15951=CARTESIAN_POINT('',(11.2119478347524,-52.3031355243012,0.));
#15952=CARTESIAN_POINT('',(214.620037028164,-9.72233226397694,0.));
#15953=CARTESIAN_POINT('',(11.4215507970056,-53.2809221054195,0.));
#15954=CARTESIAN_POINT('',(212.,15.,0.));
#15955=CARTESIAN_POINT('Origin',(212.,2.50000000000003,0.));
#15956=CARTESIAN_POINT('',(205.,15.,0.));
#15957=CARTESIAN_POINT('',(0.,15.,0.));
#15958=CARTESIAN_POINT('',(205.,13.8660254037845,0.));
#15959=CARTESIAN_POINT('',(205.,13.,0.));
#15960=CARTESIAN_POINT('',(45.2458348754007,-78.3680848350663,0.));
#15961=CARTESIAN_POINT('',(201.2,11.2320508075689,0.));
#15962=CARTESIAN_POINT('',(201.2,7.76794919243114,0.));
#15963=CARTESIAN_POINT('',(201.2,11.2320508075689,0.));
#15964=CARTESIAN_POINT('',(198.2,6.03589838486225,0.));
#15965=CARTESIAN_POINT('',(201.2,7.76794919243114,0.));
#15966=CARTESIAN_POINT('',(195.2,7.76794919243112,0.));
#15967=CARTESIAN_POINT('',(198.2,6.03589838486225,0.));
#15968=CARTESIAN_POINT('',(195.2,11.2320508075689,0.));
#15969=CARTESIAN_POINT('',(195.2,7.76794919243112,0.));
#15970=CARTESIAN_POINT('',(198.2,12.9641016151378,0.));
#15971=CARTESIAN_POINT('',(195.2,11.2320508075689,0.));
#15972=CARTESIAN_POINT('',(198.2,12.9641016151378,0.));
#15973=CARTESIAN_POINT('',(195.2,-6.23205080756882,0.));
#15974=CARTESIAN_POINT('',(195.2,-2.76794919243105,0.));
#15975=CARTESIAN_POINT('',(195.2,-2.76794919243105,0.));
#15976=CARTESIAN_POINT('',(198.2,-1.03589838486218,0.));
#15977=CARTESIAN_POINT('',(198.2,-1.03589838486218,0.));
#15978=CARTESIAN_POINT('',(201.2,-2.76794919243107,0.));
#15979=CARTESIAN_POINT('',(201.2,-2.76794919243107,0.));
#15980=CARTESIAN_POINT('',(201.2,-6.23205080756883,0.));
#15981=CARTESIAN_POINT('',(201.2,-6.23205080756883,0.));
#15982=CARTESIAN_POINT('',(198.2,-7.9641016151377,0.));
#15983=CARTESIAN_POINT('',(198.2,-7.9641016151377,0.));
#15984=CARTESIAN_POINT('',(195.2,-6.23205080756882,0.));
#15985=CARTESIAN_POINT('Origin',(11.4215507970056,-53.2809221054195,-9.));
#15986=CARTESIAN_POINT('',(190.,-15.,-9.));
#15987=CARTESIAN_POINT('',(190.,-15.,-9.));
#15988=CARTESIAN_POINT('',(214.620037028164,-9.72233226397694,-9.));
#15989=CARTESIAN_POINT('',(11.4215507970056,-53.2809221054195,-9.));
#15990=CARTESIAN_POINT('',(214.620037028164,-9.72233226397694,-9.));
#15991=CARTESIAN_POINT('Origin',(212.,2.50000000000003,-9.));
#15992=CARTESIAN_POINT('',(212.,15.,-9.));
#15993=CARTESIAN_POINT('Origin',(212.,2.50000000000003,-9.));
#15994=CARTESIAN_POINT('',(212.,15.,-9.));
#15995=CARTESIAN_POINT('Origin',(0.,15.,-9.));
#15996=CARTESIAN_POINT('',(205.,15.,10.));
#15997=CARTESIAN_POINT('',(190.,15.,10.));
#15998=CARTESIAN_POINT('',(205.,15.,0.));
#15999=CARTESIAN_POINT('',(157.,15.,-9.));
#16000=CARTESIAN_POINT('',(0.,15.,-9.));
#16001=CARTESIAN_POINT('',(157.,15.,-9.));
#16002=CARTESIAN_POINT('Origin',(155.,0.,-9.));
#16003=CARTESIAN_POINT('',(155.,13.,-9.));
#16004=CARTESIAN_POINT('',(155.,13.,0.));
#16005=CARTESIAN_POINT('',(155.,-13.,-9.));
#16006=CARTESIAN_POINT('',(155.,0.,-9.));
#16007=CARTESIAN_POINT('',(155.,-13.,-9.));
#16008=CARTESIAN_POINT('',(155.,-3.95,-1.));
#16009=CARTESIAN_POINT('',(155.,-3.95,-1.));
#16010=CARTESIAN_POINT('',(155.,3.95,-1.));
#16011=CARTESIAN_POINT('',(155.,-3.95,-1.));
#16012=CARTESIAN_POINT('',(155.,3.95,-1.));
#16013=CARTESIAN_POINT('Origin',(1.48690583655155E-15,-15.,-9.));
#16014=CARTESIAN_POINT('',(157.,-15.,-9.));
#16015=CARTESIAN_POINT('',(157.,-15.,-9.));
#16016=CARTESIAN_POINT('',(1.48690583655155E-15,-15.,-9.));
#16017=CARTESIAN_POINT('Origin',(0.,0.,-9.));
#16018=CARTESIAN_POINT('Origin',(157.,13.,-9.));
#16019=CARTESIAN_POINT('Origin',(157.,-13.,-9.));
#16020=CARTESIAN_POINT('Origin',(212.,2.50000000000003,-7.));
#16021=CARTESIAN_POINT('Origin',(212.,2.50000000000003,-8.));
#16022=CARTESIAN_POINT('Origin',(11.2119478347524,-52.3031355243012,10.));
#16023=CARTESIAN_POINT('',(195.,-12.9054582556007,10.));
#16024=CARTESIAN_POINT('',(195.,-12.9054582556007,10.));
#16025=CARTESIAN_POINT('',(11.2119478347524,-52.3031355243012,10.));
#16026=CARTESIAN_POINT('Origin',(195.,0.,10.));
#16027=CARTESIAN_POINT('',(195.,13.,10.));
#16028=CARTESIAN_POINT('',(195.,0.,10.));
#16029=CARTESIAN_POINT('',(195.,13.,10.));
#16030=CARTESIAN_POINT('Origin',(0.,0.,10.));
#16031=CARTESIAN_POINT('',(205.,13.8660254037845,10.));
#16032=CARTESIAN_POINT('',(205.,13.,10.));
#16033=CARTESIAN_POINT('',(203.5,13.,10.));
#16034=CARTESIAN_POINT('',(190.,13.,10.));
#16035=CARTESIAN_POINT('',(45.2458348754007,-78.3680848350663,10.));
#16036=CARTESIAN_POINT('Origin',(157.,-13.,-9.));
#16037=CARTESIAN_POINT('Origin',(157.,13.,-9.));
#16038=CARTESIAN_POINT('Origin',(184.75,0.,-4.6));
#16039=CARTESIAN_POINT('Origin',(164.75,0.,-4.6));
#16040=CARTESIAN_POINT('Origin',(195.2,-6.23205080756882,-3.));
#16041=CARTESIAN_POINT('',(198.2,-7.9641016151377,-3.));
#16042=CARTESIAN_POINT('',(198.2,-7.9641016151377,-3.));
#16043=CARTESIAN_POINT('',(195.2,-6.23205080756882,-3.));
#16044=CARTESIAN_POINT('',(195.2,-6.23205080756882,-3.));
#16045=CARTESIAN_POINT('',(195.2,-6.23205080756882,-3.));
#16046=CARTESIAN_POINT('Origin',(198.2,-7.9641016151377,-3.));
#16047=CARTESIAN_POINT('',(201.2,-6.23205080756883,-3.));
#16048=CARTESIAN_POINT('',(201.2,-6.23205080756883,-3.));
#16049=CARTESIAN_POINT('',(198.2,-7.9641016151377,-3.));
#16050=CARTESIAN_POINT('Origin',(201.2,-6.23205080756883,-3.));
#16051=CARTESIAN_POINT('',(201.2,-2.76794919243107,-3.));
#16052=CARTESIAN_POINT('',(201.2,-2.76794919243107,-3.));
#16053=CARTESIAN_POINT('',(201.2,-6.23205080756883,-3.));
#16054=CARTESIAN_POINT('Origin',(201.2,-2.76794919243107,-3.));
#16055=CARTESIAN_POINT('',(198.2,-1.03589838486218,-3.));
#16056=CARTESIAN_POINT('',(198.2,-1.03589838486218,-3.));
#16057=CARTESIAN_POINT('',(201.2,-2.76794919243107,-3.));
#16058=CARTESIAN_POINT('Origin',(198.2,-1.03589838486218,-3.));
#16059=CARTESIAN_POINT('',(195.2,-2.76794919243105,-3.));
#16060=CARTESIAN_POINT('',(195.2,-2.76794919243105,-3.));
#16061=CARTESIAN_POINT('',(198.2,-1.03589838486218,-3.));
#16062=CARTESIAN_POINT('Origin',(195.2,-2.76794919243105,-3.));
#16063=CARTESIAN_POINT('',(195.2,-2.76794919243105,-3.));
#16064=CARTESIAN_POINT('Origin',(0.,0.,-3.));
#16065=CARTESIAN_POINT('Origin',(198.2,12.9641016151378,-3.));
#16066=CARTESIAN_POINT('',(198.2,12.9641016151378,-3.));
#16067=CARTESIAN_POINT('',(198.2,12.9641016151378,-3.));
#16068=CARTESIAN_POINT('',(201.2,11.2320508075689,-3.));
#16069=CARTESIAN_POINT('',(198.2,12.9641016151378,-3.));
#16070=CARTESIAN_POINT('',(201.2,11.2320508075689,-3.));
#16071=CARTESIAN_POINT('Origin',(195.2,11.2320508075689,-3.));
#16072=CARTESIAN_POINT('',(195.2,11.2320508075689,-3.));
#16073=CARTESIAN_POINT('',(195.2,11.2320508075689,-3.));
#16074=CARTESIAN_POINT('',(195.2,11.2320508075689,-3.));
#16075=CARTESIAN_POINT('Origin',(195.2,7.76794919243112,-3.));
#16076=CARTESIAN_POINT('',(195.2,7.76794919243112,-3.));
#16077=CARTESIAN_POINT('',(195.2,7.76794919243112,-3.));
#16078=CARTESIAN_POINT('',(195.2,7.76794919243112,-3.));
#16079=CARTESIAN_POINT('Origin',(198.2,6.03589838486225,-3.));
#16080=CARTESIAN_POINT('',(198.2,6.03589838486225,-3.));
#16081=CARTESIAN_POINT('',(198.2,6.03589838486225,-3.));
#16082=CARTESIAN_POINT('',(198.2,6.03589838486225,-3.));
#16083=CARTESIAN_POINT('Origin',(201.2,7.76794919243114,-3.));
#16084=CARTESIAN_POINT('',(201.2,7.76794919243114,-3.));
#16085=CARTESIAN_POINT('',(201.2,7.76794919243114,-3.));
#16086=CARTESIAN_POINT('',(201.2,7.76794919243114,-3.));
#16087=CARTESIAN_POINT('Origin',(201.2,11.2320508075689,-3.));
#16088=CARTESIAN_POINT('',(201.2,11.2320508075689,-3.));
#16089=CARTESIAN_POINT('Origin',(0.,0.,-3.));
#16090=CARTESIAN_POINT('Origin',(0.,13.,0.));
#16091=CARTESIAN_POINT('',(203.5,13.,0.));
#16092=CARTESIAN_POINT('Origin',(205.,13.,0.));
#16093=CARTESIAN_POINT('',(205.,13.8660254037845,0.));
#16094=CARTESIAN_POINT('Origin',(205.,13.8660254037845,0.));
#16095=CARTESIAN_POINT('Origin',(0.,9.80814117218957E-17,-1.));
#16096=CARTESIAN_POINT('',(155.,3.95,-1.));
#16097=CARTESIAN_POINT('',(155.,-3.95,-1.));
#16098=CARTESIAN_POINT('Origin',(155.,-3.95,-1.));
#16099=CARTESIAN_POINT('Origin',(155.,3.95,-1.));
#16100=CARTESIAN_POINT('',(0.,0.,0.));
#16101=CARTESIAN_POINT('Origin',(171.5,0.,-9.));
#16102=CARTESIAN_POINT('',(167.5,4.89858719658942E-16,-4.6));
#16103=CARTESIAN_POINT('Origin',(171.5,0.,-4.6));
#16104=CARTESIAN_POINT('',(167.5,4.89858719658966E-16,-13.1339745962156));
#16105=CARTESIAN_POINT('',(167.5,4.89858719658942E-16,-9.));
#16106=CARTESIAN_POINT('',(169.886751345948,3.66024982483438,-9.));
#16107=CARTESIAN_POINT('Origin',(171.5,3.67483821150927E-13,-6.20577136594092));
#16108=CARTESIAN_POINT('',(169.886751345948,-3.66024982483438,-9.));
#16109=CARTESIAN_POINT('Origin',(171.5,0.,-9.));
#16110=CARTESIAN_POINT('Origin',(171.5,3.67483821150927E-13,-6.20577136594092));
#16111=CARTESIAN_POINT('Origin',(171.5,0.,-9.));
#16112=CARTESIAN_POINT('',(169.25,2.75545529808155E-16,-1.));
#16113=CARTESIAN_POINT('Origin',(171.5,0.,-1.));
#16114=CARTESIAN_POINT('',(169.25,2.75545529808155E-16,-4.6));
#16115=CARTESIAN_POINT('',(169.25,2.75545529808155E-16,-9.));
#16116=CARTESIAN_POINT('Origin',(171.5,0.,-4.6));
#16117=CARTESIAN_POINT('Origin',(183.5,0.,-9.));
#16118=CARTESIAN_POINT('',(179.5,4.89858719658942E-16,-4.6));
#16119=CARTESIAN_POINT('Origin',(183.5,0.,-4.6));
#16120=CARTESIAN_POINT('',(179.5,4.89858719658942E-16,-9.));
#16121=CARTESIAN_POINT('',(179.5,4.89858719658942E-16,-9.));
#16122=CARTESIAN_POINT('Origin',(183.5,0.,-9.));
#16123=CARTESIAN_POINT('Origin',(183.5,0.,-9.));
#16124=CARTESIAN_POINT('',(181.25,2.75545529808155E-16,-1.));
#16125=CARTESIAN_POINT('Origin',(183.5,0.,-1.));
#16126=CARTESIAN_POINT('',(181.25,2.75545529808155E-16,-4.6));
#16127=CARTESIAN_POINT('',(181.25,2.75545529808155E-16,-9.));
#16128=CARTESIAN_POINT('Origin',(183.5,0.,-4.6));
#16129=CARTESIAN_POINT('Origin',(210.,2.50000000000003,-9.));
#16130=CARTESIAN_POINT('',(217.,2.50000000000003,-9.));
#16131=CARTESIAN_POINT('Origin',(210.,2.50000000000003,-9.));
#16132=CARTESIAN_POINT('',(217.,2.50000000000003,-8.));
#16133=CARTESIAN_POINT('',(217.,2.50000000000003,-9.));
#16134=CARTESIAN_POINT('Origin',(210.,2.50000000000003,-8.));
#16135=CARTESIAN_POINT('Origin',(210.,2.50000000000003,-8.));
#16136=CARTESIAN_POINT('',(220.,2.50000000000003,-8.));
#16137=CARTESIAN_POINT('Origin',(210.,2.50000000000003,-8.));
#16138=CARTESIAN_POINT('',(220.,2.50000000000003,-7.));
#16139=CARTESIAN_POINT('',(220.,2.50000000000003,-8.));
#16140=CARTESIAN_POINT('Origin',(210.,2.50000000000003,-7.));
#16141=CARTESIAN_POINT('Origin',(210.,2.50000000000003,-7.));
#16142=CARTESIAN_POINT('',(221.1,2.50000000000003,-7.));
#16143=CARTESIAN_POINT('Origin',(210.,2.50000000000003,-7.));
#16144=CARTESIAN_POINT('',(221.1,2.50000000000003,0.));
#16145=CARTESIAN_POINT('',(221.1,2.50000000000003,-7.));
#16146=CARTESIAN_POINT('Origin',(210.,2.50000000000003,0.));
#16147=CARTESIAN_POINT('Origin',(160.,-15.,-3.));
#16148=CARTESIAN_POINT('',(160.,3.94999999999999,-3.));
#16149=CARTESIAN_POINT('',(190.,3.94999999999999,-3.));
#16150=CARTESIAN_POINT('',(190.,3.95,-3.));
#16151=CARTESIAN_POINT('',(190.,15.,-3.));
#16152=CARTESIAN_POINT('',(190.,-15.,-3.));
#16153=CARTESIAN_POINT('',(162.,15.,-3.));
#16154=CARTESIAN_POINT('',(160.,15.,-3.));
#16155=CARTESIAN_POINT('',(160.,13.,-3.));
#16156=CARTESIAN_POINT('Origin',(162.,13.,-3.));
#16157=CARTESIAN_POINT('',(160.,-15.,-3.));
#16158=CARTESIAN_POINT('Origin',(160.,-15.,-3.));
#16159=CARTESIAN_POINT('',(190.,-3.95,-3.));
#16160=CARTESIAN_POINT('',(160.,-3.95,-3.));
#16161=CARTESIAN_POINT('',(190.,-3.95,-3.));
#16162=CARTESIAN_POINT('',(160.,-13.,-3.));
#16163=CARTESIAN_POINT('',(160.,-15.,-3.));
#16164=CARTESIAN_POINT('',(162.,-15.,-3.));
#16165=CARTESIAN_POINT('Origin',(162.,-13.,-3.));
#16166=CARTESIAN_POINT('',(190.,-15.,-3.));
#16167=CARTESIAN_POINT('',(160.,-15.,-3.));
#16168=CARTESIAN_POINT('',(190.,-15.,-3.));
#16169=CARTESIAN_POINT('Origin',(190.,-15.,0.));
#16170=CARTESIAN_POINT('',(190.,3.95,-1.));
#16171=CARTESIAN_POINT('',(190.,3.95,-1.));
#16172=CARTESIAN_POINT('',(190.,-3.95,-1.));
#16173=CARTESIAN_POINT('',(190.,-3.95,-1.));
#16174=CARTESIAN_POINT('',(190.,-3.95,-1.));
#16175=CARTESIAN_POINT('',(190.,-15.,0.));
#16176=CARTESIAN_POINT('',(190.,-15.,0.));
#16177=CARTESIAN_POINT('',(190.,15.,0.));
#16178=CARTESIAN_POINT('',(190.,-15.,0.));
#16179=CARTESIAN_POINT('',(190.,15.,0.));
#16180=CARTESIAN_POINT('Origin',(13.1197502427733,-56.2532019429921,-9.));
#16181=CARTESIAN_POINT('',(212.839139451054,-9.67330222977594,0.));
#16182=CARTESIAN_POINT('',(13.1197502427733,-56.2532019429921,0.));
#16183=CARTESIAN_POINT('',(190.,-15.,-9.));
#16184=CARTESIAN_POINT('',(190.,-15.,-9.));
#16185=CARTESIAN_POINT('',(212.839139451054,-9.67330222977594,-9.));
#16186=CARTESIAN_POINT('',(13.1197502427733,-56.2532019429921,-9.));
#16187=CARTESIAN_POINT('',(212.839139451054,-9.67330222977594,-9.));
#16188=CARTESIAN_POINT('Origin',(210.,2.50000000000003,-9.));
#16189=CARTESIAN_POINT('',(210.,15.,0.));
#16190=CARTESIAN_POINT('Origin',(210.,2.50000000000003,0.));
#16191=CARTESIAN_POINT('',(210.,15.,-9.));
#16192=CARTESIAN_POINT('Origin',(210.,2.50000000000003,-9.));
#16193=CARTESIAN_POINT('',(210.,15.,-9.));
#16194=CARTESIAN_POINT('Origin',(0.,15.,-9.));
#16195=CARTESIAN_POINT('',(0.,15.,0.));
#16196=CARTESIAN_POINT('',(162.,15.,-9.));
#16197=CARTESIAN_POINT('',(0.,15.,-9.));
#16198=CARTESIAN_POINT('',(162.,15.,-9.));
#16199=CARTESIAN_POINT('Origin',(160.,0.,-9.));
#16200=CARTESIAN_POINT('',(160.,13.,-9.));
#16201=CARTESIAN_POINT('',(160.,13.,0.));
#16202=CARTESIAN_POINT('',(160.,7.49999999999998,-9.));
#16203=CARTESIAN_POINT('',(160.,0.,-9.));
#16204=CARTESIAN_POINT('',(160.,7.49999999999997,-15.));
#16205=CARTESIAN_POINT('',(160.,7.49999999999997,-19.));
#16206=CARTESIAN_POINT('',(160.,3.49999999999997,-19.));
#16207=CARTESIAN_POINT('Origin',(160.,3.49999999999997,-15.));
#16208=CARTESIAN_POINT('',(160.,-3.50000000000003,-19.));
#16209=CARTESIAN_POINT('',(160.,-7.50000000000003,-19.));
#16210=CARTESIAN_POINT('',(160.,-7.50000000000003,-15.));
#16211=CARTESIAN_POINT('Origin',(160.,-3.50000000000003,-15.));
#16212=CARTESIAN_POINT('',(160.,-7.50000000000002,-9.));
#16213=CARTESIAN_POINT('',(160.,-7.50000000000003,-19.));
#16214=CARTESIAN_POINT('',(160.,-13.,-9.));
#16215=CARTESIAN_POINT('',(160.,0.,-9.));
#16216=CARTESIAN_POINT('',(160.,-13.,-9.));
#16217=CARTESIAN_POINT('',(160.,-3.95,-1.));
#16218=CARTESIAN_POINT('',(160.,-3.95,-1.));
#16219=CARTESIAN_POINT('',(160.,3.95,-1.));
#16220=CARTESIAN_POINT('',(160.,-3.95,-1.));
#16221=CARTESIAN_POINT('',(160.,3.95,-1.));
#16222=CARTESIAN_POINT('Origin',(1.73472347597681E-15,-15.,-9.));
#16223=CARTESIAN_POINT('',(162.,-15.,-9.));
#16224=CARTESIAN_POINT('',(162.,-15.,-9.));
#16225=CARTESIAN_POINT('',(1.73472347597681E-15,-15.,-9.));
#16226=CARTESIAN_POINT('Origin',(0.,0.,-9.));
#16227=CARTESIAN_POINT('',(169.886751345948,7.49999999999998,-9.));
#16228=CARTESIAN_POINT('',(167.,7.49999999999998,-9.));
#16229=CARTESIAN_POINT('Origin',(162.,13.,-9.));
#16230=CARTESIAN_POINT('Origin',(162.,-13.,-9.));
#16231=CARTESIAN_POINT('',(169.886751345948,-7.50000000000002,-9.));
#16232=CARTESIAN_POINT('',(167.,-7.50000000000002,-9.));
#16233=CARTESIAN_POINT('',(169.886751345948,0.,-9.));
#16234=CARTESIAN_POINT('',(169.886751345948,0.,-9.));
#16235=CARTESIAN_POINT('Origin',(0.,0.,0.));
#16236=CARTESIAN_POINT('Origin',(210.,2.50000000000003,-7.));
#16237=CARTESIAN_POINT('Origin',(210.,2.50000000000003,-8.));
#16238=CARTESIAN_POINT('Origin',(162.,-13.,-9.));
#16239=CARTESIAN_POINT('Origin',(162.,13.,-9.));
#16240=CARTESIAN_POINT('Origin',(185.75,0.,-4.6));
#16241=CARTESIAN_POINT('Origin',(173.75,0.,-4.6));
#16242=CARTESIAN_POINT('Origin',(167.,-7.50000000000002,-19.));
#16243=CARTESIAN_POINT('',(167.,-7.50000000000002,-15.));
#16244=CARTESIAN_POINT('',(167.,-7.50000000000002,-14.));
#16245=CARTESIAN_POINT('',(167.,-7.50000000000002,-19.));
#16246=CARTESIAN_POINT('',(164.834936490539,-7.50000000000002,-17.75));
#16247=CARTESIAN_POINT('',(160.,-7.50000000000003,-15.));
#16248=CARTESIAN_POINT('Origin',(167.,-7.50000000000002,-19.));
#16249=CARTESIAN_POINT('',(167.,-3.50000000000002,-19.));
#16250=CARTESIAN_POINT('Origin',(167.,-3.50000000000002,-15.));
#16251=CARTESIAN_POINT('',(167.,3.49999999999998,-19.));
#16252=CARTESIAN_POINT('',(167.,-7.50000000000002,-19.));
#16253=CARTESIAN_POINT('',(167.,7.49999999999998,-15.));
#16254=CARTESIAN_POINT('Origin',(167.,3.49999999999998,-15.));
#16255=CARTESIAN_POINT('',(167.,7.49999999999998,-14.));
#16256=CARTESIAN_POINT('',(167.,7.49999999999998,-19.));
#16257=CARTESIAN_POINT('',(167.,-7.50000000000002,-14.));
#16258=CARTESIAN_POINT('Origin',(167.,7.49999999999998,-19.));
#16259=CARTESIAN_POINT('',(164.834936490539,7.49999999999998,-17.75));
#16260=CARTESIAN_POINT('',(167.,7.49999999999998,-15.));
#16261=CARTESIAN_POINT('Origin',(0.,0.,-19.));
#16262=CARTESIAN_POINT('',(167.,-3.50000000000002,-19.));
#16263=CARTESIAN_POINT('',(160.,3.49999999999997,-19.));
#16264=CARTESIAN_POINT('Origin',(-4.33680868994196E-16,3.49999999999995,
-15.));
#16265=CARTESIAN_POINT('Origin',(4.33680868994207E-16,-3.50000000000005,
-15.));
#16266=CARTESIAN_POINT('Origin',(167.,-7.50000000000002,-14.));
#16267=CARTESIAN_POINT('Origin',(0.,0.,-1.));
#16268=CARTESIAN_POINT('',(190.,-3.95,-1.));
#16269=CARTESIAN_POINT('',(190.,3.95,-1.));
#16270=CARTESIAN_POINT('Origin',(190.,3.95,-1.));
#16271=CARTESIAN_POINT('Origin',(190.,-3.95,-1.));
#16272=CARTESIAN_POINT('',(0.,0.,0.));
#16273=CARTESIAN_POINT('Origin',(171.5,0.,9.));
#16274=CARTESIAN_POINT('',(167.5,-4.89858719658942E-16,4.6));
#16275=CARTESIAN_POINT('Origin',(171.5,0.,4.6));
#16276=CARTESIAN_POINT('',(167.5,-4.89858719658721E-16,13.1339745962156));
#16277=CARTESIAN_POINT('',(167.5,-4.89858719658942E-16,9.));
#16278=CARTESIAN_POINT('',(169.886751345948,-3.66024982483438,9.));
#16279=CARTESIAN_POINT('Origin',(171.5,-6.00377027238687E-14,6.20577136594074));
#16280=CARTESIAN_POINT('',(169.886751345948,3.66024982483438,9.));
#16281=CARTESIAN_POINT('Origin',(171.5,0.,9.));
#16282=CARTESIAN_POINT('Origin',(171.5,-6.00377027238687E-14,6.20577136594074));
#16283=CARTESIAN_POINT('Origin',(171.5,0.,9.));
#16284=CARTESIAN_POINT('',(169.25,-2.75545529808155E-16,1.));
#16285=CARTESIAN_POINT('Origin',(171.5,0.,1.));
#16286=CARTESIAN_POINT('',(169.25,-2.75545529808155E-16,4.6));
#16287=CARTESIAN_POINT('',(169.25,-2.75545529808155E-16,9.));
#16288=CARTESIAN_POINT('Origin',(171.5,0.,4.6));
#16289=CARTESIAN_POINT('Origin',(183.5,0.,9.));
#16290=CARTESIAN_POINT('',(179.5,-4.89858719658942E-16,4.6));
#16291=CARTESIAN_POINT('Origin',(183.5,0.,4.6));
#16292=CARTESIAN_POINT('',(179.5,-4.89858719658942E-16,9.));
#16293=CARTESIAN_POINT('',(179.5,-4.89858719658942E-16,9.));
#16294=CARTESIAN_POINT('Origin',(183.5,0.,9.));
#16295=CARTESIAN_POINT('Origin',(183.5,0.,9.));
#16296=CARTESIAN_POINT('',(181.25,-2.75545529808155E-16,1.));
#16297=CARTESIAN_POINT('Origin',(183.5,0.,1.));
#16298=CARTESIAN_POINT('',(181.25,-2.75545529808155E-16,4.6));
#16299=CARTESIAN_POINT('',(181.25,-2.75545529808155E-16,9.));
#16300=CARTESIAN_POINT('Origin',(183.5,0.,4.6));
#16301=CARTESIAN_POINT('Origin',(210.,2.50000000000003,9.));
#16302=CARTESIAN_POINT('',(217.,2.50000000000003,9.));
#16303=CARTESIAN_POINT('Origin',(210.,2.50000000000003,9.));
#16304=CARTESIAN_POINT('',(217.,2.50000000000003,8.));
#16305=CARTESIAN_POINT('',(217.,2.50000000000003,9.));
#16306=CARTESIAN_POINT('Origin',(210.,2.50000000000003,8.));
#16307=CARTESIAN_POINT('Origin',(210.,2.50000000000003,8.));
#16308=CARTESIAN_POINT('',(220.,2.50000000000003,8.));
#16309=CARTESIAN_POINT('Origin',(210.,2.50000000000003,8.));
#16310=CARTESIAN_POINT('',(220.,2.50000000000003,7.));
#16311=CARTESIAN_POINT('',(220.,2.50000000000003,8.));
#16312=CARTESIAN_POINT('Origin',(210.,2.50000000000003,7.));
#16313=CARTESIAN_POINT('Origin',(210.,2.50000000000003,7.));
#16314=CARTESIAN_POINT('',(221.1,2.50000000000003,7.));
#16315=CARTESIAN_POINT('Origin',(210.,2.50000000000003,7.));
#16316=CARTESIAN_POINT('',(221.1,2.50000000000003,0.));
#16317=CARTESIAN_POINT('',(221.1,2.50000000000003,7.));
#16318=CARTESIAN_POINT('Origin',(210.,2.50000000000003,0.));
#16319=CARTESIAN_POINT('Origin',(160.,-15.,3.));
#16320=CARTESIAN_POINT('',(160.,3.94999999999999,3.));
#16321=CARTESIAN_POINT('',(190.,3.94999999999999,3.));
#16322=CARTESIAN_POINT('',(190.,3.95,3.));
#16323=CARTESIAN_POINT('',(160.,13.,3.));
#16324=CARTESIAN_POINT('',(160.,-15.,3.));
#16325=CARTESIAN_POINT('',(162.,15.,3.));
#16326=CARTESIAN_POINT('Origin',(162.,13.,3.));
#16327=CARTESIAN_POINT('',(190.,15.,3.));
#16328=CARTESIAN_POINT('',(160.,15.,3.));
#16329=CARTESIAN_POINT('',(190.,-15.,3.));
#16330=CARTESIAN_POINT('Origin',(160.,-15.,3.));
#16331=CARTESIAN_POINT('',(190.,-3.95,3.));
#16332=CARTESIAN_POINT('',(160.,-3.95,3.));
#16333=CARTESIAN_POINT('',(190.,-3.95,3.));
#16334=CARTESIAN_POINT('',(190.,-15.,3.));
#16335=CARTESIAN_POINT('',(190.,-15.,3.));
#16336=CARTESIAN_POINT('',(162.,-15.,3.));
#16337=CARTESIAN_POINT('',(160.,-15.,3.));
#16338=CARTESIAN_POINT('',(160.,-13.,3.));
#16339=CARTESIAN_POINT('Origin',(162.,-13.,3.));
#16340=CARTESIAN_POINT('',(160.,-15.,3.));
#16341=CARTESIAN_POINT('Origin',(190.,-15.,0.));
#16342=CARTESIAN_POINT('',(190.,3.95,1.));
#16343=CARTESIAN_POINT('',(190.,3.95,1.));
#16344=CARTESIAN_POINT('',(190.,15.,0.));
#16345=CARTESIAN_POINT('',(190.,15.,0.));
#16346=CARTESIAN_POINT('',(190.,-15.,0.));
#16347=CARTESIAN_POINT('',(190.,-15.,0.));
#16348=CARTESIAN_POINT('',(190.,-15.,0.));
#16349=CARTESIAN_POINT('',(190.,-3.95,1.));
#16350=CARTESIAN_POINT('',(190.,-3.95,1.));
#16351=CARTESIAN_POINT('',(190.,-3.95,1.));
#16352=CARTESIAN_POINT('Origin',(13.1197502427733,-56.2532019429921,9.));
#16353=CARTESIAN_POINT('',(212.839139451054,-9.67330222977594,0.));
#16354=CARTESIAN_POINT('',(13.1197502427733,-56.2532019429921,0.));
#16355=CARTESIAN_POINT('',(212.839139451054,-9.67330222977594,9.));
#16356=CARTESIAN_POINT('',(212.839139451054,-9.67330222977594,9.));
#16357=CARTESIAN_POINT('',(190.,-15.,9.));
#16358=CARTESIAN_POINT('',(13.1197502427733,-56.2532019429921,9.));
#16359=CARTESIAN_POINT('',(190.,-15.,9.));
#16360=CARTESIAN_POINT('Origin',(210.,2.50000000000003,9.));
#16361=CARTESIAN_POINT('',(210.,15.,0.));
#16362=CARTESIAN_POINT('Origin',(210.,2.50000000000003,0.));
#16363=CARTESIAN_POINT('',(210.,15.,9.));
#16364=CARTESIAN_POINT('',(210.,15.,9.));
#16365=CARTESIAN_POINT('Origin',(210.,2.50000000000003,9.));
#16366=CARTESIAN_POINT('Origin',(0.,15.,9.));
#16367=CARTESIAN_POINT('',(162.,15.,9.));
#16368=CARTESIAN_POINT('',(162.,15.,9.));
#16369=CARTESIAN_POINT('',(0.,15.,9.));
#16370=CARTESIAN_POINT('',(0.,15.,0.));
#16371=CARTESIAN_POINT('Origin',(160.,0.,9.));
#16372=CARTESIAN_POINT('',(160.,13.,9.));
#16373=CARTESIAN_POINT('',(160.,13.,0.));
#16374=CARTESIAN_POINT('',(160.,3.95,1.));
#16375=CARTESIAN_POINT('',(160.,3.95,1.));
#16376=CARTESIAN_POINT('',(160.,-3.95,1.));
#16377=CARTESIAN_POINT('',(160.,-3.95,1.));
#16378=CARTESIAN_POINT('',(160.,-3.95,1.));
#16379=CARTESIAN_POINT('',(160.,-13.,9.));
#16380=CARTESIAN_POINT('',(160.,-13.,9.));
#16381=CARTESIAN_POINT('',(160.,-7.50000000000002,9.));
#16382=CARTESIAN_POINT('',(160.,0.,9.));
#16383=CARTESIAN_POINT('',(160.,-7.50000000000003,15.));
#16384=CARTESIAN_POINT('',(160.,-7.50000000000003,19.));
#16385=CARTESIAN_POINT('',(160.,-3.50000000000003,19.));
#16386=CARTESIAN_POINT('Origin',(160.,-3.50000000000003,15.));
#16387=CARTESIAN_POINT('',(160.,3.49999999999997,19.));
#16388=CARTESIAN_POINT('',(160.,-7.50000000000003,19.));
#16389=CARTESIAN_POINT('',(160.,7.49999999999997,15.));
#16390=CARTESIAN_POINT('Origin',(160.,3.49999999999997,15.));
#16391=CARTESIAN_POINT('',(160.,7.49999999999998,9.));
#16392=CARTESIAN_POINT('',(160.,7.49999999999997,19.));
#16393=CARTESIAN_POINT('',(160.,0.,9.));
#16394=CARTESIAN_POINT('Origin',(1.73472347597681E-15,-15.,9.));
#16395=CARTESIAN_POINT('',(162.,-15.,9.));
#16396=CARTESIAN_POINT('',(162.,-15.,9.));
#16397=CARTESIAN_POINT('',(1.73472347597681E-15,-15.,9.));
#16398=CARTESIAN_POINT('Origin',(0.,0.,9.));
#16399=CARTESIAN_POINT('',(169.886751345948,7.49999999999998,9.));
#16400=CARTESIAN_POINT('',(167.,7.49999999999998,9.));
#16401=CARTESIAN_POINT('',(169.886751345948,0.,9.));
#16402=CARTESIAN_POINT('',(169.886751345948,-7.50000000000002,9.));
#16403=CARTESIAN_POINT('',(169.886751345948,0.,9.));
#16404=CARTESIAN_POINT('',(167.,-7.50000000000002,9.));
#16405=CARTESIAN_POINT('Origin',(162.,-13.,9.));
#16406=CARTESIAN_POINT('Origin',(162.,13.,9.));
#16407=CARTESIAN_POINT('Origin',(0.,0.,0.));
#16408=CARTESIAN_POINT('Origin',(210.,2.50000000000003,7.));
#16409=CARTESIAN_POINT('Origin',(210.,2.50000000000003,8.));
#16410=CARTESIAN_POINT('Origin',(162.,-13.,9.));
#16411=CARTESIAN_POINT('Origin',(162.,13.,9.));
#16412=CARTESIAN_POINT('Origin',(185.75,0.,4.6));
#16413=CARTESIAN_POINT('Origin',(173.75,0.,4.6));
#16414=CARTESIAN_POINT('Origin',(167.,-7.50000000000002,19.));
#16415=CARTESIAN_POINT('',(167.,-7.50000000000002,15.));
#16416=CARTESIAN_POINT('',(167.,-7.50000000000002,14.));
#16417=CARTESIAN_POINT('',(167.,-7.50000000000002,19.));
#16418=CARTESIAN_POINT('',(160.,-7.50000000000003,15.));
#16419=CARTESIAN_POINT('',(164.834936490539,-7.50000000000002,17.75));
#16420=CARTESIAN_POINT('Origin',(167.,-7.50000000000002,19.));
#16421=CARTESIAN_POINT('',(167.,7.49999999999998,14.));
#16422=CARTESIAN_POINT('',(167.,-7.50000000000002,14.));
#16423=CARTESIAN_POINT('',(167.,7.49999999999998,15.));
#16424=CARTESIAN_POINT('',(167.,7.49999999999998,19.));
#16425=CARTESIAN_POINT('',(167.,3.49999999999998,19.));
#16426=CARTESIAN_POINT('Origin',(167.,3.49999999999998,15.));
#16427=CARTESIAN_POINT('',(167.,-3.50000000000002,19.));
#16428=CARTESIAN_POINT('',(167.,-7.50000000000002,19.));
#16429=CARTESIAN_POINT('Origin',(167.,-3.50000000000002,15.));
#16430=CARTESIAN_POINT('Origin',(167.,7.49999999999998,19.));
#16431=CARTESIAN_POINT('',(167.,7.49999999999998,15.));
#16432=CARTESIAN_POINT('',(164.834936490539,7.49999999999998,17.75));
#16433=CARTESIAN_POINT('Origin',(0.,0.,19.));
#16434=CARTESIAN_POINT('',(160.,3.49999999999997,19.));
#16435=CARTESIAN_POINT('',(167.,-3.50000000000002,19.));
#16436=CARTESIAN_POINT('Origin',(-4.33680868994196E-16,3.49999999999995,
15.));
#16437=CARTESIAN_POINT('Origin',(4.33680868994207E-16,-3.50000000000005,
15.));
#16438=CARTESIAN_POINT('Origin',(167.,-7.50000000000002,14.));
#16439=CARTESIAN_POINT('Origin',(0.,0.,1.));
#16440=CARTESIAN_POINT('',(190.,3.95,1.));
#16441=CARTESIAN_POINT('',(190.,-3.95,1.));
#16442=CARTESIAN_POINT('Origin',(190.,3.95,1.));
#16443=CARTESIAN_POINT('Origin',(190.,-3.95,1.));
#16444=CARTESIAN_POINT('',(0.,0.,0.));
#16445=CARTESIAN_POINT('Origin',(9.,9.25,5.));
#16446=CARTESIAN_POINT('',(6.,9.25,1.6));
#16447=CARTESIAN_POINT('Origin',(9.,9.25,1.6));
#16448=CARTESIAN_POINT('',(6.,9.25,5.));
#16449=CARTESIAN_POINT('',(6.,9.25,5.));
#16450=CARTESIAN_POINT('Origin',(9.,9.25,5.));
#16451=CARTESIAN_POINT('Origin',(9.,-9.25,5.));
#16452=CARTESIAN_POINT('',(6.,-9.25,1.6));
#16453=CARTESIAN_POINT('Origin',(9.,-9.25,1.6));
#16454=CARTESIAN_POINT('',(6.,-9.25,5.));
#16455=CARTESIAN_POINT('',(6.,-9.25,5.));
#16456=CARTESIAN_POINT('Origin',(9.,-9.25,5.));
#16457=CARTESIAN_POINT('Origin',(15.7,41.,5.));
#16458=CARTESIAN_POINT('',(12.45,41.,1.6));
#16459=CARTESIAN_POINT('Origin',(15.7,41.,1.6));
#16460=CARTESIAN_POINT('',(12.45,41.,5.));
#16461=CARTESIAN_POINT('',(12.45,41.,5.));
#16462=CARTESIAN_POINT('Origin',(15.7,41.,5.));
#16463=CARTESIAN_POINT('Origin',(15.7,27.,5.));
#16464=CARTESIAN_POINT('',(12.45,27.,1.6));
#16465=CARTESIAN_POINT('Origin',(15.7,27.,1.6));
#16466=CARTESIAN_POINT('',(12.45,27.,5.));
#16467=CARTESIAN_POINT('',(12.45,27.,5.));
#16468=CARTESIAN_POINT('Origin',(15.7,27.,5.));
#16469=CARTESIAN_POINT('Origin',(-0.5,0.,5.));
#16470=CARTESIAN_POINT('',(1.75,-2.75545529808155E-16,5.));
#16471=CARTESIAN_POINT('Origin',(-0.5,0.,5.));
#16472=CARTESIAN_POINT('',(1.75,-2.75545529808155E-16,0.499999999999999));
#16473=CARTESIAN_POINT('',(1.75,-2.75545529808155E-16,5.));
#16474=CARTESIAN_POINT('Origin',(-0.5,0.,0.5));
#16475=CARTESIAN_POINT('Origin',(9.,-9.25,-5.));
#16476=CARTESIAN_POINT('',(7.25,-9.25,0.499999999999999));
#16477=CARTESIAN_POINT('Origin',(9.,-9.25,0.5));
#16478=CARTESIAN_POINT('',(7.25,-9.25,1.6));
#16479=CARTESIAN_POINT('',(7.25,-9.25,-5.));
#16480=CARTESIAN_POINT('Origin',(9.,-9.25,1.6));
#16481=CARTESIAN_POINT('Origin',(9.,9.25,-5.));
#16482=CARTESIAN_POINT('',(7.25,9.25,0.499999999999999));
#16483=CARTESIAN_POINT('Origin',(9.,9.25,0.5));
#16484=CARTESIAN_POINT('',(7.25,9.25,1.6));
#16485=CARTESIAN_POINT('',(7.25,9.25,-5.));
#16486=CARTESIAN_POINT('Origin',(9.,9.25,1.6));
#16487=CARTESIAN_POINT('Origin',(-11.25,0.,0.));
#16488=CARTESIAN_POINT('',(-14.25,-3.67394039744206E-16,0.5));
#16489=CARTESIAN_POINT('Origin',(-11.25,0.,0.5));
#16490=CARTESIAN_POINT('',(-14.25,-3.67394039744206E-16,5.));
#16491=CARTESIAN_POINT('',(-14.25,-3.67394039744206E-16,0.));
#16492=CARTESIAN_POINT('Origin',(-11.25,0.,5.));
#16493=CARTESIAN_POINT('Origin',(15.7,41.,5.));
#16494=CARTESIAN_POINT('',(14.2,41.,0.499999999999999));
#16495=CARTESIAN_POINT('Origin',(15.7,41.,0.5));
#16496=CARTESIAN_POINT('',(14.2,41.,1.6));
#16497=CARTESIAN_POINT('',(14.2,41.,5.));
#16498=CARTESIAN_POINT('Origin',(15.7,41.,1.6));
#16499=CARTESIAN_POINT('Origin',(15.7,27.,5.));
#16500=CARTESIAN_POINT('',(14.2,27.,0.499999999999999));
#16501=CARTESIAN_POINT('Origin',(15.7,27.,0.5));
#16502=CARTESIAN_POINT('',(14.2,27.,1.6));
#16503=CARTESIAN_POINT('',(14.2,27.,5.));
#16504=CARTESIAN_POINT('Origin',(15.7,27.,1.6));
#16505=CARTESIAN_POINT('Origin',(20.,46.5,5.));
#16506=CARTESIAN_POINT('',(20.,42.5,0.5));
#16507=CARTESIAN_POINT('',(20.,21.5710678118655,0.5));
#16508=CARTESIAN_POINT('',(20.,42.5,0.5));
#16509=CARTESIAN_POINT('',(20.,42.5,5.));
#16510=CARTESIAN_POINT('',(20.,42.5,5.));
#16511=CARTESIAN_POINT('',(20.,21.5710678118655,5.));
#16512=CARTESIAN_POINT('',(20.,34.,5.));
#16513=CARTESIAN_POINT('',(20.,21.5710678118655,0.));
#16514=CARTESIAN_POINT('Origin',(-12.5,46.5,5.));
#16515=CARTESIAN_POINT('',(-8.5,46.5,0.5));
#16516=CARTESIAN_POINT('',(16.,46.5,0.5));
#16517=CARTESIAN_POINT('',(-8.5,46.5,0.5));
#16518=CARTESIAN_POINT('',(-8.5,46.5,5.));
#16519=CARTESIAN_POINT('',(-8.5,46.5,5.));
#16520=CARTESIAN_POINT('',(16.,46.5,5.));
#16521=CARTESIAN_POINT('',(-12.5,46.5,5.));
#16522=CARTESIAN_POINT('',(16.,46.5,5.));
#16523=CARTESIAN_POINT('Origin',(-12.5,0.,5.));
#16524=CARTESIAN_POINT('',(-12.5,28.5710678118655,0.5));
#16525=CARTESIAN_POINT('',(-12.5,42.5,0.5));
#16526=CARTESIAN_POINT('',(-12.5,28.5710678118655,0.5));
#16527=CARTESIAN_POINT('',(-12.5,28.5710678118655,5.));
#16528=CARTESIAN_POINT('',(-12.5,28.5710678118655,5.));
#16529=CARTESIAN_POINT('',(-12.5,42.5,5.));
#16530=CARTESIAN_POINT('',(-12.5,0.,5.));
#16531=CARTESIAN_POINT('',(-12.5,42.5,5.));
#16532=CARTESIAN_POINT('Origin',(-8.5,42.5,5.));
#16533=CARTESIAN_POINT('Origin',(-8.5,42.5,0.5));
#16534=CARTESIAN_POINT('Origin',(-8.5,42.5,5.));
#16535=CARTESIAN_POINT('Origin',(16.,42.5,5.));
#16536=CARTESIAN_POINT('Origin',(16.,42.5,0.5));
#16537=CARTESIAN_POINT('Origin',(16.,42.5,5.));
#16538=CARTESIAN_POINT('Origin',(0.,40.5,0.));
#16539=CARTESIAN_POINT('',(-4.,40.5,0.5));
#16540=CARTESIAN_POINT('',(-4.,40.5,5.));
#16541=CARTESIAN_POINT('',(-4.,40.5,0.));
#16542=CARTESIAN_POINT('',(4.,40.5,0.5));
#16543=CARTESIAN_POINT('',(0.,40.5,0.5));
#16544=CARTESIAN_POINT('',(4.,40.5,5.));
#16545=CARTESIAN_POINT('',(4.,40.5,0.));
#16546=CARTESIAN_POINT('',(0.,40.5,5.));
#16547=CARTESIAN_POINT('Origin',(4.,37.5,0.));
#16548=CARTESIAN_POINT('',(7.,37.5,0.5));
#16549=CARTESIAN_POINT('Origin',(4.,37.5,0.5));
#16550=CARTESIAN_POINT('',(7.,37.5,5.));
#16551=CARTESIAN_POINT('',(7.,37.5,0.));
#16552=CARTESIAN_POINT('Origin',(4.,37.5,5.));
#16553=CARTESIAN_POINT('Origin',(7.,1.01192202765314E-15,0.));
#16554=CARTESIAN_POINT('',(7.,25.5,0.5));
#16555=CARTESIAN_POINT('',(7.,1.01192202765314E-15,0.5));
#16556=CARTESIAN_POINT('',(7.,25.5,5.));
#16557=CARTESIAN_POINT('',(7.,25.5,0.));
#16558=CARTESIAN_POINT('',(7.,1.01192202765314E-15,5.));
#16559=CARTESIAN_POINT('Origin',(4.,25.5,0.));
#16560=CARTESIAN_POINT('',(4.,22.5,0.5));
#16561=CARTESIAN_POINT('Origin',(4.,25.5,0.5));
#16562=CARTESIAN_POINT('',(4.,22.5,5.));
#16563=CARTESIAN_POINT('',(4.,22.5,0.));
#16564=CARTESIAN_POINT('Origin',(4.,25.5,5.));
#16565=CARTESIAN_POINT('Origin',(0.,22.5,0.));
#16566=CARTESIAN_POINT('',(-4.,22.5,0.5));
#16567=CARTESIAN_POINT('',(0.,22.5,0.5));
#16568=CARTESIAN_POINT('',(-4.,22.5,5.));
#16569=CARTESIAN_POINT('',(-4.,22.5,0.));
#16570=CARTESIAN_POINT('',(0.,22.5,5.));
#16571=CARTESIAN_POINT('Origin',(-4.,25.5,0.));
#16572=CARTESIAN_POINT('',(-7.,25.5,0.5));
#16573=CARTESIAN_POINT('Origin',(-4.,25.5,0.5));
#16574=CARTESIAN_POINT('',(-7.,25.5,5.));
#16575=CARTESIAN_POINT('',(-7.,25.5,0.));
#16576=CARTESIAN_POINT('Origin',(-4.,25.5,5.));
#16577=CARTESIAN_POINT('Origin',(-7.,-1.01192202765314E-15,0.));
#16578=CARTESIAN_POINT('',(-7.,37.5,0.5));
#16579=CARTESIAN_POINT('',(-7.,-1.01192202765314E-15,0.5));
#16580=CARTESIAN_POINT('',(-7.,37.5,5.));
#16581=CARTESIAN_POINT('',(-7.,37.5,0.));
#16582=CARTESIAN_POINT('',(-7.,-1.01192202765314E-15,5.));
#16583=CARTESIAN_POINT('Origin',(-4.,37.5,0.));
#16584=CARTESIAN_POINT('Origin',(-4.,37.5,0.5));
#16585=CARTESIAN_POINT('Origin',(-4.,37.5,5.));
#16586=CARTESIAN_POINT('Origin',(-22.5,-2.69181229030884E-15,0.));
#16587=CARTESIAN_POINT('',(-22.5,14.4289321881346,5.));
#16588=CARTESIAN_POINT('',(-22.5,14.4289321881346,0.5));
#16589=CARTESIAN_POINT('',(-22.5,14.4289321881346,0.));
#16590=CARTESIAN_POINT('',(-22.5,-7.5,0.5));
#16591=CARTESIAN_POINT('',(-22.5,-7.5,0.5));
#16592=CARTESIAN_POINT('',(-22.5,-7.5,5.));
#16593=CARTESIAN_POINT('',(-22.5,-7.5,0.));
#16594=CARTESIAN_POINT('',(-22.5,-2.69181229030884E-15,5.));
#16595=CARTESIAN_POINT('Origin',(-19.5,19.5,0.));
#16596=CARTESIAN_POINT('',(-13.9644660940673,25.0355339059327,5.));
#16597=CARTESIAN_POINT('',(-13.9644660940673,25.0355339059327,0.5));
#16598=CARTESIAN_POINT('',(-13.9644660940673,25.0355339059327,0.));
#16599=CARTESIAN_POINT('',(-21.0355339059327,17.9644660940673,0.5));
#16600=CARTESIAN_POINT('',(-21.0355339059327,17.9644660940673,0.5));
#16601=CARTESIAN_POINT('',(-21.0355339059327,17.9644660940673,5.));
#16602=CARTESIAN_POINT('',(-21.0355339059327,17.9644660940673,0.));
#16603=CARTESIAN_POINT('',(-19.5,19.5,5.));
#16604=CARTESIAN_POINT('Origin',(0.,-12.5,0.));
#16605=CARTESIAN_POINT('',(-17.5,-12.5,5.));
#16606=CARTESIAN_POINT('',(-17.5,-12.5,0.5));
#16607=CARTESIAN_POINT('',(-17.5,-12.5,0.));
#16608=CARTESIAN_POINT('',(9.5,-12.5,0.5));
#16609=CARTESIAN_POINT('',(9.5,-12.5,0.5));
#16610=CARTESIAN_POINT('',(9.5,-12.5,5.));
#16611=CARTESIAN_POINT('',(9.5,-12.5,0.));
#16612=CARTESIAN_POINT('',(0.,-12.5,5.));
#16613=CARTESIAN_POINT('Origin',(14.5,0.,0.));
#16614=CARTESIAN_POINT('',(14.5,-7.5,5.));
#16615=CARTESIAN_POINT('',(14.5,-7.5,0.5));
#16616=CARTESIAN_POINT('',(14.5,-7.5,0.));
#16617=CARTESIAN_POINT('',(14.5,11.9289321881345,0.5));
#16618=CARTESIAN_POINT('',(14.5,11.9289321881345,0.5));
#16619=CARTESIAN_POINT('',(14.5,11.9289321881345,5.));
#16620=CARTESIAN_POINT('',(14.5,11.9289321881345,5.));
#16621=CARTESIAN_POINT('',(14.5,0.,5.));
#16622=CARTESIAN_POINT('Origin',(0.249999999999984,-0.249999999999985,0.));
#16623=CARTESIAN_POINT('',(15.9644660940673,15.4644660940673,5.));
#16624=CARTESIAN_POINT('',(15.9644660940673,15.4644660940673,0.5));
#16625=CARTESIAN_POINT('',(15.9644660940673,15.4644660940673,0.));
#16626=CARTESIAN_POINT('',(18.5355339059327,18.0355339059327,0.5));
#16627=CARTESIAN_POINT('',(18.5355339059327,18.0355339059327,0.5));
#16628=CARTESIAN_POINT('',(18.5355339059327,18.0355339059327,5.));
#16629=CARTESIAN_POINT('',(18.5355339059327,18.0355339059327,5.));
#16630=CARTESIAN_POINT('',(0.249999999999984,-0.249999999999985,5.));
#16631=CARTESIAN_POINT('Origin',(15.,21.5710678118655,5.));
#16632=CARTESIAN_POINT('Origin',(15.,21.5710678118655,0.5));
#16633=CARTESIAN_POINT('Origin',(15.,21.5710678118655,5.));
#16634=CARTESIAN_POINT('Origin',(19.5,11.9289321881345,0.));
#16635=CARTESIAN_POINT('Origin',(19.5,11.9289321881345,0.5));
#16636=CARTESIAN_POINT('Origin',(19.5,11.9289321881345,5.));
#16637=CARTESIAN_POINT('Origin',(9.5,-7.5,0.));
#16638=CARTESIAN_POINT('Origin',(9.5,-7.5,0.5));
#16639=CARTESIAN_POINT('Origin',(9.5,-7.5,5.));
#16640=CARTESIAN_POINT('Origin',(-17.5,-7.5,0.));
#16641=CARTESIAN_POINT('Origin',(-17.5,-7.5,0.5));
#16642=CARTESIAN_POINT('Origin',(-17.5,-7.5,5.));
#16643=CARTESIAN_POINT('Origin',(-17.5,14.4289321881346,0.));
#16644=CARTESIAN_POINT('Origin',(-17.5,14.4289321881346,0.5));
#16645=CARTESIAN_POINT('Origin',(-17.5,14.4289321881346,5.));
#16646=CARTESIAN_POINT('Origin',(-17.5,28.5710678118655,5.));
#16647=CARTESIAN_POINT('Origin',(-17.5,28.5710678118655,0.5));
#16648=CARTESIAN_POINT('Origin',(-17.5,28.5710678118655,5.));
#16649=CARTESIAN_POINT('Origin',(0.,1.64743813908221E-15,5.));
#16650=CARTESIAN_POINT('Origin',(17.2,27.,1.6));
#16651=CARTESIAN_POINT('Origin',(17.2,41.,1.6));
#16652=CARTESIAN_POINT('Origin',(16.,42.5,0.5));
#16653=CARTESIAN_POINT('Origin',(10.5,-9.25,1.6));
#16654=CARTESIAN_POINT('Origin',(10.5,9.25,1.6));
#16655=CARTESIAN_POINT('',(0.,0.,0.));
#16656=CARTESIAN_POINT('Origin',(3.,0.,0.));
#16657=CARTESIAN_POINT('',(3.,-8.57252759403147E-16,-7.));
#16658=CARTESIAN_POINT('Origin',(3.,0.,0.));
#16659=CARTESIAN_POINT('',(3.5,-7.9602041944578E-16,-6.5));
#16660=CARTESIAN_POINT('Origin',(3.,-7.9602041944578E-16,-6.5));
#16661=CARTESIAN_POINT('Origin',(3.5,0.,0.));
#16662=CARTESIAN_POINT('Origin',(2.,0.,0.));
#16663=CARTESIAN_POINT('',(2.,8.57252759403147E-16,-7.));
#16664=CARTESIAN_POINT('',(2.,-8.57252759403147E-16,7.));
#16665=CARTESIAN_POINT('Origin',(2.,0.,0.));
#16666=CARTESIAN_POINT('Origin',(2.,0.,0.));
#16667=CARTESIAN_POINT('',(1.5,-7.9602041944578E-16,6.5));
#16668=CARTESIAN_POINT('Origin',(2.,-7.9602041944578E-16,6.5));
#16669=CARTESIAN_POINT('Origin',(1.5,0.,0.));
#16670=CARTESIAN_POINT('Origin',(-2.,0.,0.));
#16671=CARTESIAN_POINT('',(-2.,-8.57252759403147E-16,-7.));
#16672=CARTESIAN_POINT('Origin',(-2.,0.,0.));
#16673=CARTESIAN_POINT('',(-1.5,-7.9602041944578E-16,-6.5));
#16674=CARTESIAN_POINT('Origin',(-2.,-7.9602041944578E-16,-6.5));
#16675=CARTESIAN_POINT('Origin',(-1.5,0.,0.));
#16676=CARTESIAN_POINT('Origin',(-3.,0.,0.));
#16677=CARTESIAN_POINT('',(-3.,8.57252759403147E-16,-7.));
#16678=CARTESIAN_POINT('',(-3.,-8.57252759403147E-16,7.));
#16679=CARTESIAN_POINT('Origin',(-3.,0.,0.));
#16680=CARTESIAN_POINT('Origin',(-3.,0.,0.));
#16681=CARTESIAN_POINT('',(-3.5,-7.9602041944578E-16,6.5));
#16682=CARTESIAN_POINT('Origin',(-3.,-7.9602041944578E-16,6.5));
#16683=CARTESIAN_POINT('Origin',(-3.5,0.,0.));
#16684=CARTESIAN_POINT('Origin',(-3.5,0.,0.));
#16685=CARTESIAN_POINT('',(-3.5,-8.57252759403147E-16,-7.));
#16686=CARTESIAN_POINT('Origin',(-3.5,0.,0.));
#16687=CARTESIAN_POINT('',(-1.5,-6.12323399573677E-16,-5.));
#16688=CARTESIAN_POINT('Origin',(-1.5,0.,0.));
#16689=CARTESIAN_POINT('',(1.5,-6.12323399573677E-16,-5.));
#16690=CARTESIAN_POINT('',(-3.5,-6.12323399573677E-16,-5.));
#16691=CARTESIAN_POINT('Origin',(1.5,0.,0.));
#16692=CARTESIAN_POINT('Origin',(-3.5,0.,0.));
#16693=CARTESIAN_POINT('',(-3.5,-8.57252759403147E-16,-7.));
#16694=CARTESIAN_POINT('Origin',(-1.5,7.,0.));
#16695=CARTESIAN_POINT('Origin',(1.5,5.,0.));
#16696=CARTESIAN_POINT('Origin',(3.5,7.,0.));
#16697=CARTESIAN_POINT('',(3.5,-1.81383571472171,-2.));
#16698=CARTESIAN_POINT('',(3.5,-1.81383571472171,2.));
#16699=CARTESIAN_POINT('Origin',(3.5,0.,0.));
#16700=CARTESIAN_POINT('',(3.5,1.81383571472171,2.));
#16701=CARTESIAN_POINT('',(3.5,7.,2.));
#16702=CARTESIAN_POINT('',(3.5,1.81383571472171,-2.));
#16703=CARTESIAN_POINT('Origin',(3.5,0.,0.));
#16704=CARTESIAN_POINT('',(3.5,7.,-2.));
#16705=CARTESIAN_POINT('Origin',(-3.5,0.,0.));
#16706=CARTESIAN_POINT('',(-3.5,1.81383571472171,2.));
#16707=CARTESIAN_POINT('',(-3.5,1.81383571472171,-2.));
#16708=CARTESIAN_POINT('Origin',(-3.5,0.,0.));
#16709=CARTESIAN_POINT('',(-3.5,-1.81383571472171,2.));
#16710=CARTESIAN_POINT('',(-3.5,0.,2.));
#16711=CARTESIAN_POINT('',(-3.5,-1.81383571472171,-2.));
#16712=CARTESIAN_POINT('Origin',(-3.5,0.,0.));
#16713=CARTESIAN_POINT('',(-3.5,-9.563840109097E-16,-2.));
#16714=CARTESIAN_POINT('Origin',(6.5,0.,2.));
#16715=CARTESIAN_POINT('',(6.5,-1.81383571472171,2.));
#16716=CARTESIAN_POINT('',(6.5,1.81383571472171,2.));
#16717=CARTESIAN_POINT('Origin',(6.5,0.,0.));
#16718=CARTESIAN_POINT('',(6.5,-1.81383571472171,-2.));
#16719=CARTESIAN_POINT('Origin',(6.5,-9.563840109097E-16,-2.));
#16720=CARTESIAN_POINT('',(6.5,1.81383571472171,-2.));
#16721=CARTESIAN_POINT('Origin',(6.5,0.,0.));
#16722=CARTESIAN_POINT('',(0.,0.,0.));
#16723=CARTESIAN_POINT('Origin',(3.5,0.,0.));
#16724=CARTESIAN_POINT('',(3.5,-4.89858719658941E-16,-4.));
#16725=CARTESIAN_POINT('Origin',(3.5,0.,0.));
#16726=CARTESIAN_POINT('',(-3.5,-4.89858719658941E-16,-4.));
#16727=CARTESIAN_POINT('',(3.5,-4.89858719658941E-16,-4.));
#16728=CARTESIAN_POINT('Origin',(-3.5,0.,0.));
#16729=CARTESIAN_POINT('Origin',(3.,0.,0.));
#16730=CARTESIAN_POINT('',(3.,-1.46957615897682E-15,-12.));
#16731=CARTESIAN_POINT('Origin',(3.,0.,0.));
#16732=CARTESIAN_POINT('',(3.5,-1.40834381901946E-15,-11.5));
#16733=CARTESIAN_POINT('Origin',(3.,-1.40834381901946E-15,-11.5));
#16734=CARTESIAN_POINT('Origin',(3.5,0.,0.));
#16735=CARTESIAN_POINT('Origin',(2.,0.,0.));
#16736=CARTESIAN_POINT('',(2.,1.46957615897682E-15,-12.));
#16737=CARTESIAN_POINT('',(2.,-1.46957615897682E-15,12.));
#16738=CARTESIAN_POINT('Origin',(2.,0.,0.));
#16739=CARTESIAN_POINT('Origin',(2.,0.,0.));
#16740=CARTESIAN_POINT('',(1.5,-1.40834381901946E-15,11.5));
#16741=CARTESIAN_POINT('Origin',(2.,-1.40834381901946E-15,11.5));
#16742=CARTESIAN_POINT('Origin',(1.5,0.,0.));
#16743=CARTESIAN_POINT('Origin',(-2.,0.,0.));
#16744=CARTESIAN_POINT('',(-2.,-1.46957615897682E-15,-12.));
#16745=CARTESIAN_POINT('Origin',(-2.,0.,0.));
#16746=CARTESIAN_POINT('',(-1.5,-1.40834381901946E-15,-11.5));
#16747=CARTESIAN_POINT('Origin',(-2.,-1.40834381901946E-15,-11.5));
#16748=CARTESIAN_POINT('Origin',(-1.5,0.,0.));
#16749=CARTESIAN_POINT('Origin',(-3.,0.,0.));
#16750=CARTESIAN_POINT('',(-3.,1.46957615897682E-15,-12.));
#16751=CARTESIAN_POINT('',(-3.,-1.46957615897682E-15,12.));
#16752=CARTESIAN_POINT('Origin',(-3.,0.,0.));
#16753=CARTESIAN_POINT('Origin',(-3.,0.,0.));
#16754=CARTESIAN_POINT('',(-3.5,-1.40834381901946E-15,11.5));
#16755=CARTESIAN_POINT('Origin',(-3.,-1.40834381901946E-15,11.5));
#16756=CARTESIAN_POINT('Origin',(-3.5,0.,0.));
#16757=CARTESIAN_POINT('Origin',(-3.5,0.,0.));
#16758=CARTESIAN_POINT('',(-3.5,-1.46957615897682E-15,-12.));
#16759=CARTESIAN_POINT('Origin',(-3.5,0.,0.));
#16760=CARTESIAN_POINT('',(-1.5,-1.22464679914735E-15,-10.));
#16761=CARTESIAN_POINT('Origin',(-1.5,0.,0.));
#16762=CARTESIAN_POINT('',(1.5,-1.22464679914735E-15,-10.));
#16763=CARTESIAN_POINT('',(-3.5,-1.22464679914735E-15,-10.));
#16764=CARTESIAN_POINT('Origin',(1.5,0.,0.));
#16765=CARTESIAN_POINT('Origin',(-3.5,0.,0.));
#16766=CARTESIAN_POINT('',(-3.5,-1.46957615897682E-15,-12.));
#16767=CARTESIAN_POINT('Origin',(3.5,12.,0.));
#16768=CARTESIAN_POINT('Origin',(-3.5,0.,0.));
#16769=CARTESIAN_POINT('Origin',(-1.5,12.,0.));
#16770=CARTESIAN_POINT('Origin',(1.5,10.,0.));
#16771=CARTESIAN_POINT('',(0.,0.,0.));
#16772=CARTESIAN_POINT('Origin',(22.,11.3156378831472,-20.3));
#16773=CARTESIAN_POINT('',(23.8,11.3156378831472,-20.5));
#16774=CARTESIAN_POINT('Origin',(22.,11.3156378831472,-20.5));
#16775=CARTESIAN_POINT('',(24.,11.3156378831472,-20.3));
#16776=CARTESIAN_POINT('Origin',(23.8,11.3156378831472,-20.3));
#16777=CARTESIAN_POINT('',(20.,11.3156378831472,-20.3));
#16778=CARTESIAN_POINT('Origin',(22.,11.3156378831472,-20.3));
#16779=CARTESIAN_POINT('Origin',(22.,11.3156378831472,-20.3));
#16780=CARTESIAN_POINT('Origin',(22.,11.3156378831472,-20.5));
#16781=CARTESIAN_POINT('',(20.,11.3156378831472,-18.5));
#16782=CARTESIAN_POINT('Origin',(22.,11.3156378831472,-18.5));
#16783=CARTESIAN_POINT('',(20.,11.3156378831472,-20.5));
#16784=CARTESIAN_POINT('Origin',(35.,2.,4.24264068711929));
#16785=CARTESIAN_POINT('',(36.,2.,0.));
#16786=CARTESIAN_POINT('Origin',(35.,2.,0.));
#16787=CARTESIAN_POINT('',(36.,2.,-18.5));
#16788=CARTESIAN_POINT('',(36.,2.,4.24264068711929));
#16789=CARTESIAN_POINT('Origin',(35.,2.,-18.5));
#16790=CARTESIAN_POINT('Origin',(35.,20.5,4.24264068711929));
#16791=CARTESIAN_POINT('',(36.,20.5,0.));
#16792=CARTESIAN_POINT('Origin',(35.,20.5,0.));
#16793=CARTESIAN_POINT('',(36.,20.5,-18.5));
#16794=CARTESIAN_POINT('',(36.,20.5,4.24264068711929));
#16795=CARTESIAN_POINT('Origin',(35.,20.5,-18.5));
#16796=CARTESIAN_POINT('Origin',(31.5,2.,4.24264068711929));
#16797=CARTESIAN_POINT('',(33.,2.,0.));
#16798=CARTESIAN_POINT('Origin',(31.5,2.,0.));
#16799=CARTESIAN_POINT('',(33.,2.,-18.5));
#16800=CARTESIAN_POINT('',(33.,2.,4.24264068711929));
#16801=CARTESIAN_POINT('Origin',(31.5,2.,-18.5));
#16802=CARTESIAN_POINT('Origin',(31.5,20.5,4.24264068711929));
#16803=CARTESIAN_POINT('',(33.,20.5,0.));
#16804=CARTESIAN_POINT('Origin',(31.5,20.5,0.));
#16805=CARTESIAN_POINT('',(33.,20.5,-18.5));
#16806=CARTESIAN_POINT('',(33.,20.5,4.24264068711929));
#16807=CARTESIAN_POINT('Origin',(31.5,20.5,-18.5));
#16808=CARTESIAN_POINT('Origin',(-2.25,11.5,-28.501));
#16809=CARTESIAN_POINT('',(-3.25,11.5,-10.75));
#16810=CARTESIAN_POINT('Origin',(-2.25,11.5,-10.75));
#16811=CARTESIAN_POINT('',(-3.25,11.5,-7.75));
#16812=CARTESIAN_POINT('',(-3.25,11.5,-28.501));
#16813=CARTESIAN_POINT('Origin',(-2.25,11.5,-7.75));
#16814=CARTESIAN_POINT('Origin',(11.25,11.3156378831472,-28.5));
#16815=CARTESIAN_POINT('',(8.5,11.3156378831472,-18.5));
#16816=CARTESIAN_POINT('Origin',(11.25,11.3156378831472,-18.5));
#16817=CARTESIAN_POINT('',(8.5,11.3156378831472,-28.5));
#16818=CARTESIAN_POINT('',(8.5,11.3156378831472,-28.5));
#16819=CARTESIAN_POINT('',(9.12867965644036,9.56563788314719,-28.5));
#16820=CARTESIAN_POINT('Origin',(11.25,11.3156378831472,-28.5));
#16821=CARTESIAN_POINT('',(9.12867965644036,9.56563788314719,-20.5));
#16822=CARTESIAN_POINT('',(9.12867965644036,9.56563788314719,-28.5));
#16823=CARTESIAN_POINT('',(13.3713203435596,9.56563788314719,-20.5));
#16824=CARTESIAN_POINT('Origin',(11.25,11.3156378831472,-20.5));
#16825=CARTESIAN_POINT('',(13.3713203435596,9.56563788314719,-28.5));
#16826=CARTESIAN_POINT('',(13.3713203435596,9.56563788314719,-28.5));
#16827=CARTESIAN_POINT('',(13.3713203435596,13.0656378831472,-28.5));
#16828=CARTESIAN_POINT('Origin',(11.25,11.3156378831472,-28.5));
#16829=CARTESIAN_POINT('',(13.3713203435596,13.0656378831472,-20.5));
#16830=CARTESIAN_POINT('',(13.3713203435596,13.0656378831472,-28.5));
#16831=CARTESIAN_POINT('',(9.12867965644036,13.0656378831472,-20.5));
#16832=CARTESIAN_POINT('Origin',(11.25,11.3156378831472,-20.5));
#16833=CARTESIAN_POINT('',(9.12867965644036,13.0656378831472,-28.5));
#16834=CARTESIAN_POINT('',(9.12867965644036,13.0656378831472,-28.5));
#16835=CARTESIAN_POINT('Origin',(11.25,11.3156378831472,-28.5));
#16836=CARTESIAN_POINT('Origin',(60.5,11.2499999999998,-9.0000000000003));
#16837=CARTESIAN_POINT('',(60.5,18.236594306241,-1.5));
#16838=CARTESIAN_POINT('',(60.5,17.6580028089882,-17.0000000000006));
#16839=CARTESIAN_POINT('Origin',(60.5,11.2499999999998,-9.0000000000003));
#16840=CARTESIAN_POINT('',(62.,17.6188696014285,-3.));
#16841=CARTESIAN_POINT('Ctrl Pts',(60.5,18.2365943062411,-1.5));
#16842=CARTESIAN_POINT('Ctrl Pts',(60.6825097737065,18.2365943062411,-1.5));
#16843=CARTESIAN_POINT('Ctrl Pts',(60.8626262952116,18.2235187999567,-1.5333052678753));
#16844=CARTESIAN_POINT('Ctrl Pts',(61.2066214067746,18.1719078689624,-1.66370550137199));
#16845=CARTESIAN_POINT('Ctrl Pts',(61.3654081421642,18.1331565114149,-1.76128416762843));
#16846=CARTESIAN_POINT('Ctrl Pts',(61.6474355482113,18.0314004414372,-2.01416097458981));
#16847=CARTESIAN_POINT('Ctrl Pts',(61.7642104747049,17.9678801157231,-2.17047440300412));
#16848=CARTESIAN_POINT('Ctrl Pts',(61.8976884723899,17.8548001066011,-2.44379950745487));
#16849=CARTESIAN_POINT('Ctrl Pts',(61.9354353141332,17.8102641486262,-2.55046487110271));
#16850=CARTESIAN_POINT('Ctrl Pts',(61.9865427819248,17.7176723731834,-2.76979605527032));
#16851=CARTESIAN_POINT('Ctrl Pts',(61.999575711242,17.6697427007191,-2.88213719062229));
#16852=CARTESIAN_POINT('Ctrl Pts',(61.999996602987,17.6204611304348,-2.99631374883044));
#16853=CARTESIAN_POINT('Ctrl Pts',(62.,17.6196654289333,-2.99815690123519));
#16854=CARTESIAN_POINT('Ctrl Pts',(62.,17.6188696014285,-3.));
#16855=CARTESIAN_POINT('',(62.,17.10768725693,-15.5000000000006));
#16856=CARTESIAN_POINT('Origin',(62.,11.2499999999998,-9.0000000000003));
#16857=CARTESIAN_POINT('Ctrl Pts',(60.5,17.6580028089882,-17.0000000000006));
#16858=CARTESIAN_POINT('Ctrl Pts',(60.6849224319866,17.6580028089882,-17.0000000000006));
#16859=CARTESIAN_POINT('Ctrl Pts',(60.8675370698961,17.6460282159484,-16.9658078455989));
#16860=CARTESIAN_POINT('Ctrl Pts',(61.2149045564291,17.5988242934699,-16.8321104937404));
#16861=CARTESIAN_POINT('Ctrl Pts',(61.3748310905333,17.563515359271,-16.732437992471));
#16862=CARTESIAN_POINT('Ctrl Pts',(61.6563081266554,17.4712622036046,-16.4754110401718));
#16863=CARTESIAN_POINT('Ctrl Pts',(61.772057271832,17.4141013272841,-16.317682393564));
#16864=CARTESIAN_POINT('Ctrl Pts',(61.9020528190627,17.3133591165629,-16.0445469649045));
#16865=CARTESIAN_POINT('Ctrl Pts',(61.9381950183413,17.2744715583663,-15.9400312132836));
#16866=CARTESIAN_POINT('Ctrl Pts',(61.9870959225303,17.1937377924364,-15.7253060054237));
#16867=CARTESIAN_POINT('Ctrl Pts',(61.9995824894263,17.1520226081444,-15.6154644316008));
#16868=CARTESIAN_POINT('Ctrl Pts',(61.9999965682669,17.1091102687603,-15.5037050301089));
#16869=CARTESIAN_POINT('Ctrl Pts',(62.,17.1083988194954,-15.5018524937658));
#16870=CARTESIAN_POINT('Ctrl Pts',(62.,17.10768725693,-15.5000000000006));
#16871=CARTESIAN_POINT('Origin',(62.,11.2500000000003,-9.00000000000028));
#16872=CARTESIAN_POINT('',(60.5,4.84199719101188,-17.0000000000006));
#16873=CARTESIAN_POINT('',(60.5,4.26340569375895,-1.5));
#16874=CARTESIAN_POINT('Origin',(60.5,11.2500000000003,-9.00000000000028));
#16875=CARTESIAN_POINT('',(48.,4.26340569375895,-1.5));
#16876=CARTESIAN_POINT('',(62.,4.26340569375895,-1.5));
#16877=CARTESIAN_POINT('',(48.,4.84199719101187,-17.0000000000006));
#16878=CARTESIAN_POINT('Origin',(48.,11.2500000000003,-9.00000000000028));
#16879=CARTESIAN_POINT('',(62.,4.84199719101188,-17.0000000000006));
#16880=CARTESIAN_POINT('Origin',(48.,11.25,-9.25));
#16881=CARTESIAN_POINT('',(48.,3.88029851350817,-0.75));
#16882=CARTESIAN_POINT('',(48.,4.84687576256716,-18.5));
#16883=CARTESIAN_POINT('Origin',(48.,11.25,-9.25));
#16884=CARTESIAN_POINT('',(37.,3.88029851350817,-0.75));
#16885=CARTESIAN_POINT('',(48.,3.88029851350817,-0.75));
#16886=CARTESIAN_POINT('',(37.,0.,-9.25));
#16887=CARTESIAN_POINT('Origin',(37.,11.25,-9.25));
#16888=CARTESIAN_POINT('',(37.,4.84687576256715,-18.5));
#16889=CARTESIAN_POINT('Origin',(37.,11.25,-9.25));
#16890=CARTESIAN_POINT('',(48.,4.84687576256716,-18.5));
#16891=CARTESIAN_POINT('Origin',(11.25,11.3156378831472,10.));
#16892=CARTESIAN_POINT('',(14.,11.3156378831472,0.));
#16893=CARTESIAN_POINT('Origin',(11.25,11.3156378831472,0.));
#16894=CARTESIAN_POINT('',(14.,11.3156378831472,10.));
#16895=CARTESIAN_POINT('',(14.,11.3156378831472,10.));
#16896=CARTESIAN_POINT('',(13.3713203435596,9.56563788314719,10.));
#16897=CARTESIAN_POINT('Origin',(11.25,11.3156378831472,10.));
#16898=CARTESIAN_POINT('',(13.3713203435596,9.56563788314719,2.));
#16899=CARTESIAN_POINT('',(13.3713203435596,9.56563788314719,10.));
#16900=CARTESIAN_POINT('',(9.12867965644036,9.56563788314719,2.));
#16901=CARTESIAN_POINT('Origin',(11.25,11.3156378831472,2.));
#16902=CARTESIAN_POINT('',(9.12867965644036,9.56563788314719,10.));
#16903=CARTESIAN_POINT('',(9.12867965644036,9.56563788314719,10.));
#16904=CARTESIAN_POINT('',(9.12867965644036,13.0656378831472,10.));
#16905=CARTESIAN_POINT('Origin',(11.25,11.3156378831472,10.));
#16906=CARTESIAN_POINT('',(9.12867965644036,13.0656378831472,2.));
#16907=CARTESIAN_POINT('',(9.12867965644036,13.0656378831472,10.));
#16908=CARTESIAN_POINT('',(13.3713203435596,13.0656378831472,2.));
#16909=CARTESIAN_POINT('Origin',(11.25,11.3156378831472,2.));
#16910=CARTESIAN_POINT('',(13.3713203435596,13.0656378831472,10.));
#16911=CARTESIAN_POINT('',(13.3713203435596,13.0656378831472,10.));
#16912=CARTESIAN_POINT('Origin',(11.25,11.3156378831472,10.));
#16913=CARTESIAN_POINT('Origin',(3.,19.5,-18.5));
#16914=CARTESIAN_POINT('',(37.,0.,-18.5));
#16915=CARTESIAN_POINT('',(37.,0.,-18.5));
#16916=CARTESIAN_POINT('',(3.,0.,-18.5));
#16917=CARTESIAN_POINT('',(3.,0.,-18.5));
#16918=CARTESIAN_POINT('',(0.,3.,-18.5));
#16919=CARTESIAN_POINT('Origin',(3.,3.,-18.5));
#16920=CARTESIAN_POINT('',(4.33680868994202E-16,19.5,-18.5));
#16921=CARTESIAN_POINT('',(0.,3.,-18.5));
#16922=CARTESIAN_POINT('',(3.,22.5,-18.5));
#16923=CARTESIAN_POINT('Origin',(3.,19.5,-18.5));
#16924=CARTESIAN_POINT('',(37.,22.5,-18.5));
#16925=CARTESIAN_POINT('',(3.,22.5,-18.5));
#16926=CARTESIAN_POINT('',(37.,17.6531242374329,-18.5));
#16927=CARTESIAN_POINT('',(37.,0.,-18.5));
#16928=CARTESIAN_POINT('',(48.,17.6531242374329,-18.5));
#16929=CARTESIAN_POINT('',(48.,17.6531242374329,-18.5));
#16930=CARTESIAN_POINT('',(48.,3.39234813079909E-15,-18.5));
#16931=CARTESIAN_POINT('Origin',(0.,3.,-18.5));
#16932=CARTESIAN_POINT('',(4.33680868994202E-16,19.5,0.));
#16933=CARTESIAN_POINT('',(0.,3.,0.));
#16934=CARTESIAN_POINT('',(0.,3.,0.));
#16935=CARTESIAN_POINT('',(4.33680868994202E-16,19.5,-18.5));
#16936=CARTESIAN_POINT('',(0.,3.,-18.5));
#16937=CARTESIAN_POINT('',(0.,9.,-10.75));
#16938=CARTESIAN_POINT('',(0.,9.,-7.75));
#16939=CARTESIAN_POINT('',(0.,9.,-10.75));
#16940=CARTESIAN_POINT('',(0.,14.,-10.75));
#16941=CARTESIAN_POINT('',(0.,14.,-10.75));
#16942=CARTESIAN_POINT('',(0.,14.,-7.75));
#16943=CARTESIAN_POINT('',(0.,14.,-10.75));
#16944=CARTESIAN_POINT('',(0.,14.,-7.75));
#16945=CARTESIAN_POINT('Origin',(11.25,11.3156378831472,10.));
#16946=CARTESIAN_POINT('',(14.4729344439275,9.56563788314719,10.));
#16947=CARTESIAN_POINT('',(14.4729344439275,13.0656378831472,10.));
#16948=CARTESIAN_POINT('Origin',(48.,11.25,-9.25));
#16949=CARTESIAN_POINT('',(48.,18.6197014864918,-0.75));
#16950=CARTESIAN_POINT('Origin',(48.,11.25,-9.25));
#16951=CARTESIAN_POINT('',(48.,-0.293389173340333,-0.75));
#16952=CARTESIAN_POINT('',(48.,18.236594306241,-1.5));
#16953=CARTESIAN_POINT('',(48.,18.236594306241,-1.5));
#16954=CARTESIAN_POINT('',(48.,17.6580028089882,-17.0000000000006));
#16955=CARTESIAN_POINT('Origin',(48.,11.2499999999998,-9.0000000000003));
#16956=CARTESIAN_POINT('',(48.,4.84199719101188,-17.0000000000006));
#16957=CARTESIAN_POINT('Origin',(48.,11.25,-9.25));
#16958=CARTESIAN_POINT('',(37.,22.5,-9.25));
#16959=CARTESIAN_POINT('Origin',(37.,11.25,-9.25));
#16960=CARTESIAN_POINT('',(37.,18.6197014864918,-0.75));
#16961=CARTESIAN_POINT('Origin',(37.,11.25,-9.25));
#16962=CARTESIAN_POINT('',(48.,18.6197014864918,-0.75));
#16963=CARTESIAN_POINT('Origin',(37.,0.,-18.5));
#16964=CARTESIAN_POINT('',(37.,0.,-18.5));
#16965=CARTESIAN_POINT('Origin',(37.,0.,-18.5));
#16966=CARTESIAN_POINT('',(37.,22.5,0.));
#16967=CARTESIAN_POINT('',(37.,22.5,-18.5));
#16968=CARTESIAN_POINT('',(37.,0.,0.));
#16969=CARTESIAN_POINT('',(37.,0.,0.));
#16970=CARTESIAN_POINT('',(37.,0.,-18.5));
#16971=CARTESIAN_POINT('',(37.,-0.293389173340335,-0.75));
#16972=CARTESIAN_POINT('Origin',(37.,0.,-18.5));
#16973=CARTESIAN_POINT('',(37.,22.5,-18.5));
#16974=CARTESIAN_POINT('Origin',(3.,0.,-18.5));
#16975=CARTESIAN_POINT('',(3.,0.,0.));
#16976=CARTESIAN_POINT('',(3.,0.,0.));
#16977=CARTESIAN_POINT('',(3.,0.,-18.5));
#16978=CARTESIAN_POINT('Origin',(3.,3.,-18.5));
#16979=CARTESIAN_POINT('Origin',(3.,3.,0.));
#16980=CARTESIAN_POINT('Origin',(3.,19.5,-18.5));
#16981=CARTESIAN_POINT('',(3.,22.5,0.));
#16982=CARTESIAN_POINT('Origin',(3.,19.5,0.));
#16983=CARTESIAN_POINT('',(3.,22.5,-18.5));
#16984=CARTESIAN_POINT('Origin',(3.,22.5,-18.5));
#16985=CARTESIAN_POINT('',(3.,22.5,0.));
#16986=CARTESIAN_POINT('Origin',(3.,19.5,0.));
#16987=CARTESIAN_POINT('Origin',(37.,-0.293389173340335,-0.75));
#16988=CARTESIAN_POINT('Origin',(62.,11.2499999999998,-9.0000000000003));
#16989=CARTESIAN_POINT('',(62.,18.236594306241,-1.5));
#16990=CARTESIAN_POINT('',(62.,17.6580028089882,-17.0000000000006));
#16991=CARTESIAN_POINT('Origin',(62.,18.236594306241,-1.5));
#16992=CARTESIAN_POINT('',(60.5,18.236594306241,-1.5));
#16993=CARTESIAN_POINT('Origin',(62.,4.84199719101188,-17.0000000000006));
#16994=CARTESIAN_POINT('',(60.5,4.84199719101188,-17.0000000000006));
#16995=CARTESIAN_POINT('Origin',(62.,11.2499999999998,-9.0000000000003));
#16996=CARTESIAN_POINT('',(62.,4.88113039857151,-3.));
#16997=CARTESIAN_POINT('',(62.,5.39231274307003,-15.5000000000006));
#16998=CARTESIAN_POINT('Origin',(62.,11.2500000000003,-9.00000000000028));
#16999=CARTESIAN_POINT('',(62.,17.6580028089882,-15.5000000000006));
#17000=CARTESIAN_POINT('',(62.,4.26340569375895,-3.));
#17001=CARTESIAN_POINT('Origin',(60.5,11.2499999999998,-3.));
#17002=CARTESIAN_POINT('Ctrl Pts',(62.,4.8811303985715,-3.));
#17003=CARTESIAN_POINT('Ctrl Pts',(62.,4.88033457106672,-2.99815690123521));
#17004=CARTESIAN_POINT('Ctrl Pts',(61.999996602987,4.87953886956515,-2.99631374883042));
#17005=CARTESIAN_POINT('Ctrl Pts',(61.999575711242,4.8302572992812,-2.88213719062315));
#17006=CARTESIAN_POINT('Ctrl Pts',(61.9865427819249,4.78232762681674,-2.76979605527046));
#17007=CARTESIAN_POINT('Ctrl Pts',(61.9354353141332,4.68973585137378,-2.55046487110269));
#17008=CARTESIAN_POINT('Ctrl Pts',(61.8976884723899,4.64519989339895,-2.44379950745486));
#17009=CARTESIAN_POINT('Ctrl Pts',(61.7642104747049,4.53211988427689,-2.17047440300411));
#17010=CARTESIAN_POINT('Ctrl Pts',(61.6474355482113,4.46859955856276,-2.01416097458981));
#17011=CARTESIAN_POINT('Ctrl Pts',(61.3654081421642,4.3668434885851,-1.76128416762844));
#17012=CARTESIAN_POINT('Ctrl Pts',(61.2066214067746,4.32809213103761,-1.66370550137199));
#17013=CARTESIAN_POINT('Ctrl Pts',(60.8626262952117,4.27648120004334,-1.5333052678753));
#17014=CARTESIAN_POINT('Ctrl Pts',(60.6825097737065,4.26340569375894,-1.5));
#17015=CARTESIAN_POINT('Ctrl Pts',(60.5,4.26340569375894,-1.5));
#17016=CARTESIAN_POINT('Origin',(60.5,11.2500000000003,-9.00000000000028));
#17017=CARTESIAN_POINT('Ctrl Pts',(62.,5.39231274307,-15.5000000000005));
#17018=CARTESIAN_POINT('Ctrl Pts',(62.,5.39160118050427,-15.5018524937667));
#17019=CARTESIAN_POINT('Ctrl Pts',(61.9999965682669,5.39088973123915,-15.5037050301105));
#17020=CARTESIAN_POINT('Ctrl Pts',(61.9995824894261,5.34797739185418,-15.6154644316047));
#17021=CARTESIAN_POINT('Ctrl Pts',(61.9870959225299,5.30626220756289,-15.7253060054257));
#17022=CARTESIAN_POINT('Ctrl Pts',(61.938195018341,5.22552844163345,-15.9400312132845));
#17023=CARTESIAN_POINT('Ctrl Pts',(61.9020528190626,5.186640883437,-16.0445469649049));
#17024=CARTESIAN_POINT('Ctrl Pts',(61.772057271832,5.08589867271599,-16.317682393564));
#17025=CARTESIAN_POINT('Ctrl Pts',(61.6563081266553,5.02873779639548,-16.4754110401719));
#17026=CARTESIAN_POINT('Ctrl Pts',(61.3748310905333,4.93648464072909,-16.732437992471));
#17027=CARTESIAN_POINT('Ctrl Pts',(61.2149045564291,4.90117570653016,-16.8321104937404));
#17028=CARTESIAN_POINT('Ctrl Pts',(60.8675370698961,4.85397178405163,-16.9658078455989));
#17029=CARTESIAN_POINT('Ctrl Pts',(60.6849224319866,4.84199719101184,-17.0000000000006));
#17030=CARTESIAN_POINT('Ctrl Pts',(60.5,4.84199719101184,-17.0000000000006));
#17031=CARTESIAN_POINT('Origin',(60.5,11.2499999999998,-15.5000000000006));
#17032=CARTESIAN_POINT('Origin',(11.25,11.3156378831472,-28.5));
#17033=CARTESIAN_POINT('',(11.25,9.56563788314719,-28.5));
#17034=CARTESIAN_POINT('',(11.25,13.0656378831472,-28.5));
#17035=CARTESIAN_POINT('Origin',(14.4729344439275,13.0656378831472,-20.5));
#17036=CARTESIAN_POINT('',(14.4729344439275,13.0656378831472,-20.5));
#17037=CARTESIAN_POINT('Origin',(14.4729344439275,13.0656378831472,-20.5));
#17038=CARTESIAN_POINT('Origin',(14.4729344439275,7.8996035579007,-20.5));
#17039=CARTESIAN_POINT('',(14.4729344439275,9.56563788314719,-20.5));
#17040=CARTESIAN_POINT('Origin',(14.4729344439275,9.56563788314719,-20.5));
#17041=CARTESIAN_POINT('Origin',(14.4729344439275,13.0656378831472,2.));
#17042=CARTESIAN_POINT('',(14.4729344439275,13.0656378831472,2.));
#17043=CARTESIAN_POINT('Origin',(14.4729344439275,13.0656378831472,2.));
#17044=CARTESIAN_POINT('Origin',(14.4729344439275,9.56563788314719,2.));
#17045=CARTESIAN_POINT('',(14.4729344439275,9.56563788314719,2.));
#17046=CARTESIAN_POINT('Origin',(14.4729344439275,7.8996035579007,2.));
#17047=CARTESIAN_POINT('Origin',(-4.5,14.,-10.75));
#17048=CARTESIAN_POINT('',(-4.5,9.,-10.75));
#17049=CARTESIAN_POINT('',(-4.5,9.,-10.75));
#17050=CARTESIAN_POINT('',(-4.5,14.,-10.75));
#17051=CARTESIAN_POINT('',(-4.5,14.,-10.75));
#17052=CARTESIAN_POINT('',(-4.5,14.,-10.75));
#17053=CARTESIAN_POINT('Origin',(-4.5,9.,-10.75));
#17054=CARTESIAN_POINT('',(-4.5,9.,-7.75));
#17055=CARTESIAN_POINT('',(-4.5,9.,-7.75));
#17056=CARTESIAN_POINT('',(-4.5,9.,-10.75));
#17057=CARTESIAN_POINT('Origin',(-4.5,14.,-7.75));
#17058=CARTESIAN_POINT('',(-4.5,14.,-7.75));
#17059=CARTESIAN_POINT('',(-4.5,14.,-7.75));
#17060=CARTESIAN_POINT('',(-4.5,14.,-7.75));
#17061=CARTESIAN_POINT('Origin',(-4.5,14.,-10.75));
#17062=CARTESIAN_POINT('',(-4.5,14.,-10.75));
#17063=CARTESIAN_POINT('Origin',(-4.5,9.,-10.75));
#17064=CARTESIAN_POINT('Origin',(22.,11.3156378831472,-20.5));
#17065=CARTESIAN_POINT('',(0.,0.,0.));
#17066=CARTESIAN_POINT('Origin',(-53.,0.,1.));
#17067=CARTESIAN_POINT('',(-53.4716981132075,4.97770036161242,1.));
#17068=CARTESIAN_POINT('',(-53.4716981132075,-4.97770036161242,1.));
#17069=CARTESIAN_POINT('Origin',(-53.,0.,1.));
#17070=CARTESIAN_POINT('',(-53.4716981132075,-4.97770036161242,-1.));
#17071=CARTESIAN_POINT('',(-53.4716981132075,-4.97770036161242,1.));
#17072=CARTESIAN_POINT('',(-53.4716981132075,4.97770036161242,-1.));
#17073=CARTESIAN_POINT('Origin',(-53.,0.,-1.));
#17074=CARTESIAN_POINT('',(-53.4716981132075,4.97770036161242,1.));
#17075=CARTESIAN_POINT('Origin',(-53.,0.,1.));
#17076=CARTESIAN_POINT('',(-53.5660377358491,5.97324043393491,1.));
#17077=CARTESIAN_POINT('',(-53.5660377358491,-5.97324043393491,1.));
#17078=CARTESIAN_POINT('Origin',(-53.,0.,1.));
#17079=CARTESIAN_POINT('',(-53.5660377358491,5.97324043393491,-1.));
#17080=CARTESIAN_POINT('',(-53.5660377358491,5.97324043393491,1.));
#17081=CARTESIAN_POINT('',(-53.5660377358491,-5.97324043393491,-1.));
#17082=CARTESIAN_POINT('Origin',(-53.,0.,-1.));
#17083=CARTESIAN_POINT('',(-53.5660377358491,-5.97324043393491,1.));
#17084=CARTESIAN_POINT('Origin',(-53.,0.,1.));
#17085=CARTESIAN_POINT('',(-1.0377358490566,-10.9509407955473,1.));
#17086=CARTESIAN_POINT('',(-1.0377358490566,-10.9509407955473,1.));
#17087=CARTESIAN_POINT('',(-1.03773584905659,10.9509407955473,1.));
#17088=CARTESIAN_POINT('Origin',(0.,0.,1.));
#17089=CARTESIAN_POINT('',(-53.5660377358491,5.97324043393491,1.));
#17090=CARTESIAN_POINT('',(-0.943396226415095,-9.95540072322485,1.));
#17091=CARTESIAN_POINT('',(-0.943396226415095,-9.95540072322485,1.));
#17092=CARTESIAN_POINT('',(-0.943396226415094,9.95540072322485,1.));
#17093=CARTESIAN_POINT('',(-53.4716981132075,4.97770036161242,1.));
#17094=CARTESIAN_POINT('Origin',(0.,0.,1.));
#17095=CARTESIAN_POINT('Origin',(-53.,0.,-1.));
#17096=CARTESIAN_POINT('',(-1.03773584905659,10.9509407955473,-1.));
#17097=CARTESIAN_POINT('',(-53.5660377358491,5.97324043393491,-1.));
#17098=CARTESIAN_POINT('',(-1.0377358490566,-10.9509407955473,-1.));
#17099=CARTESIAN_POINT('Origin',(0.,0.,-1.));
#17100=CARTESIAN_POINT('',(-1.0377358490566,-10.9509407955473,-1.));
#17101=CARTESIAN_POINT('',(-0.943396226415095,-9.95540072322485,-1.));
#17102=CARTESIAN_POINT('',(-0.943396226415095,-9.95540072322485,-1.));
#17103=CARTESIAN_POINT('',(-0.943396226415092,9.95540072322485,-1.));
#17104=CARTESIAN_POINT('Origin',(0.,0.,-1.));
#17105=CARTESIAN_POINT('',(-53.4716981132075,4.97770036161242,-1.));
#17106=CARTESIAN_POINT('Origin',(-1.0377358490566,-10.9509407955473,1.));
#17107=CARTESIAN_POINT('',(-1.0377358490566,-10.9509407955473,1.));
#17108=CARTESIAN_POINT('Origin',(0.,0.,1.));
#17109=CARTESIAN_POINT('',(-1.03773584905659,10.9509407955473,1.));
#17110=CARTESIAN_POINT('Origin',(-53.5660377358491,5.97324043393491,1.));
#17111=CARTESIAN_POINT('Origin',(-0.943396226415095,-9.95540072322485,1.));
#17112=CARTESIAN_POINT('',(-0.943396226415095,-9.95540072322485,1.));
#17113=CARTESIAN_POINT('Origin',(0.,0.,1.));
#17114=CARTESIAN_POINT('',(-0.943396226415092,9.95540072322485,1.));
#17115=CARTESIAN_POINT('Origin',(-53.4716981132075,4.97770036161242,1.));
#17116=CARTESIAN_POINT('',(0.,0.,0.));
#17117=CARTESIAN_POINT('Origin',(-211.,0.,35.));
#17118=CARTESIAN_POINT('',(-211.,12.7,35.));
#17119=CARTESIAN_POINT('',(-213.674620604119,-12.4151683284611,35.));
#17120=CARTESIAN_POINT('Origin',(-211.,0.,35.));
#17121=CARTESIAN_POINT('',(-213.674620604119,-12.4151683284611,-35.));
#17122=CARTESIAN_POINT('',(-213.674620604119,-12.4151683284611,35.));
#17123=CARTESIAN_POINT('',(-211.,12.7,-35.));
#17124=CARTESIAN_POINT('Origin',(-211.,0.,-35.));
#17125=CARTESIAN_POINT('',(-211.,12.7,35.));
#17126=CARTESIAN_POINT('Origin',(-211.,0.,35.));
#17127=CARTESIAN_POINT('',(-211.,14.7,35.));
#17128=CARTESIAN_POINT('',(-214.095820699256,-14.3703129471164,35.));
#17129=CARTESIAN_POINT('Origin',(-211.,0.,35.));
#17130=CARTESIAN_POINT('',(-211.,14.7,-35.));
#17131=CARTESIAN_POINT('',(-211.,14.7,35.));
#17132=CARTESIAN_POINT('',(-214.095820699256,-14.3703129471164,-35.));
#17133=CARTESIAN_POINT('Origin',(-211.,0.,-35.));
#17134=CARTESIAN_POINT('',(-214.095820699256,-14.3703129471164,35.));
#17135=CARTESIAN_POINT('Origin',(-211.,0.,35.));
#17136=CARTESIAN_POINT('',(-191.212988467299,-19.2999999999999,35.));
#17137=CARTESIAN_POINT('',(-191.212988467299,-19.2999999999999,35.));
#17138=CARTESIAN_POINT('',(189.195995188445,-19.2999999999999,35.));
#17139=CARTESIAN_POINT('',(189.195995188445,-19.2999999999999,35.));
#17140=CARTESIAN_POINT('',(213.853723455684,-14.4203419667661,35.));
#17141=CARTESIAN_POINT('',(189.195995188445,-19.2999999999999,35.));
#17142=CARTESIAN_POINT('',(211.,14.7000000000001,35.));
#17143=CARTESIAN_POINT('Origin',(211.,5.16800949240183E-14,35.));
#17144=CARTESIAN_POINT('',(-211.,14.7,35.));
#17145=CARTESIAN_POINT('',(-191.,-17.2999999999999,35.));
#17146=CARTESIAN_POINT('',(-191.,-17.2999999999999,35.));
#17147=CARTESIAN_POINT('',(211.,12.7000000000001,35.));
#17148=CARTESIAN_POINT('',(-211.,12.7,35.));
#17149=CARTESIAN_POINT('',(213.465461761033,-12.4583906787707,35.));
#17150=CARTESIAN_POINT('Origin',(211.,5.16800949240183E-14,35.));
#17151=CARTESIAN_POINT('',(189.,-17.2999999999999,35.));
#17152=CARTESIAN_POINT('',(189.,-17.2999999999999,35.));
#17153=CARTESIAN_POINT('',(189.,-17.2999999999999,35.));
#17154=CARTESIAN_POINT('Origin',(-211.,0.,-35.));
#17155=CARTESIAN_POINT('',(211.,14.7000000000001,-35.));
#17156=CARTESIAN_POINT('',(-211.,14.7,-35.));
#17157=CARTESIAN_POINT('',(213.853723455684,-14.4203419667661,-35.));
#17158=CARTESIAN_POINT('Origin',(211.,5.16800949240183E-14,-35.));
#17159=CARTESIAN_POINT('',(189.195995188445,-19.2999999999999,-35.));
#17160=CARTESIAN_POINT('',(189.195995188445,-19.2999999999999,-35.));
#17161=CARTESIAN_POINT('',(-191.212988467299,-19.2999999999999,-35.));
#17162=CARTESIAN_POINT('',(189.195995188445,-19.2999999999999,-35.));
#17163=CARTESIAN_POINT('',(-191.212988467299,-19.2999999999999,-35.));
#17164=CARTESIAN_POINT('',(-191.,-17.2999999999999,-35.));
#17165=CARTESIAN_POINT('',(-191.,-17.2999999999999,-35.));
#17166=CARTESIAN_POINT('',(189.,-17.2999999999999,-35.));
#17167=CARTESIAN_POINT('',(189.,-17.2999999999999,-35.));
#17168=CARTESIAN_POINT('',(213.465461761033,-12.4583906787707,-35.));
#17169=CARTESIAN_POINT('',(189.,-17.2999999999999,-35.));
#17170=CARTESIAN_POINT('',(211.,12.7000000000001,-35.));
#17171=CARTESIAN_POINT('Origin',(211.,5.16800949240183E-14,-35.));
#17172=CARTESIAN_POINT('',(-211.,12.7,-35.));
#17173=CARTESIAN_POINT('Origin',(-191.212988467299,-19.2999999999999,35.));
#17174=CARTESIAN_POINT('',(-191.212988467299,-19.2999999999999,35.));
#17175=CARTESIAN_POINT('Origin',(189.195995188445,-19.2999999999999,35.));
#17176=CARTESIAN_POINT('',(189.195995188445,-19.2999999999999,35.));
#17177=CARTESIAN_POINT('Origin',(189.195995188445,-19.2999999999999,35.));
#17178=CARTESIAN_POINT('',(213.853723455684,-14.4203419667661,35.));
#17179=CARTESIAN_POINT('Origin',(211.,5.16800949240183E-14,35.));
#17180=CARTESIAN_POINT('',(211.,14.7000000000001,35.));
#17181=CARTESIAN_POINT('Origin',(-211.,14.7,35.));
#17182=CARTESIAN_POINT('Origin',(-191.,-17.2999999999999,35.));
#17183=CARTESIAN_POINT('',(-191.,-17.2999999999999,35.));
#17184=CARTESIAN_POINT('Origin',(189.,-17.2999999999999,35.));
#17185=CARTESIAN_POINT('',(189.,-17.2999999999999,35.));
#17186=CARTESIAN_POINT('Origin',(189.,-17.2999999999999,35.));
#17187=CARTESIAN_POINT('',(213.465461761033,-12.4583906787707,35.));
#17188=CARTESIAN_POINT('Origin',(211.,5.16800949240183E-14,35.));
#17189=CARTESIAN_POINT('',(211.,12.7000000000001,35.));
#17190=CARTESIAN_POINT('Origin',(-211.,12.7,35.));
#17191=CARTESIAN_POINT('',(0.,0.,0.));
#17192=CARTESIAN_POINT('Origin',(96.5599999999999,35.0599999999999,380.));
#17193=CARTESIAN_POINT('',(93.2794382684679,36.6601295965039,380.));
#17194=CARTESIAN_POINT('',(93.279438268468,33.4598704034959,380.));
#17195=CARTESIAN_POINT('Origin',(96.5599999999999,35.0599999999999,380.));
#17196=CARTESIAN_POINT('',(93.279438268468,33.4598704034959,0.));
#17197=CARTESIAN_POINT('',(93.279438268468,33.4598704034959,380.));
#17198=CARTESIAN_POINT('',(93.2794382684679,36.6601295965039,0.));
#17199=CARTESIAN_POINT('Origin',(96.5599999999999,35.0599999999999,0.));
#17200=CARTESIAN_POINT('',(93.2794382684679,36.6601295965039,380.));
#17201=CARTESIAN_POINT('Origin',(104.609999923724,22.4600011663401,380.));
#17202=CARTESIAN_POINT('',(95.6600000543452,29.0599999999999,380.));
#17203=CARTESIAN_POINT('',(96.5599999999999,29.5751481628425,380.));
#17204=CARTESIAN_POINT('',(95.6600000543452,29.0599999999999,380.));
#17205=CARTESIAN_POINT('',(97.4599999456547,29.0599999999999,380.));
#17206=CARTESIAN_POINT('',(96.5599999999999,29.5751481628425,380.));
#17207=CARTESIAN_POINT('',(100.764466193213,29.0599999999999,380.));
#17208=CARTESIAN_POINT('',(97.4599999456547,29.0599999999999,380.));
#17209=CARTESIAN_POINT('',(104.810000327124,25.0100007629401,380.));
#17210=CARTESIAN_POINT('',(100.764466193213,29.0599999999999,380.));
#17211=CARTESIAN_POINT('',(104.810000327124,22.4600011663401,380.));
#17212=CARTESIAN_POINT('',(104.810000327124,25.0100007629401,380.));
#17213=CARTESIAN_POINT('',(104.609999923724,22.2600007629398,380.));
#17214=CARTESIAN_POINT('Origin',(104.609999923724,22.4600011663401,380.));
#17215=CARTESIAN_POINT('',(101.210000196921,22.2600007629398,380.));
#17216=CARTESIAN_POINT('',(104.609999923724,22.2600007629398,380.));
#17217=CARTESIAN_POINT('',(100.61,21.6600005660189,380.));
#17218=CARTESIAN_POINT('Origin',(101.210000196921,21.6600005660189,380.));
#17219=CARTESIAN_POINT('',(100.61,20.7600003735979,380.));
#17220=CARTESIAN_POINT('',(100.61,21.6600005660189,380.));
#17221=CARTESIAN_POINT('',(100.810000373598,20.5599999999999,380.));
#17222=CARTESIAN_POINT('Origin',(100.810000373598,20.7600003735979,380.));
#17223=CARTESIAN_POINT('',(100.910000144262,20.5599999999999,380.));
#17224=CARTESIAN_POINT('',(100.810000373598,20.5599999999999,380.));
#17225=CARTESIAN_POINT('',(101.109999564186,20.3600005800758,380.));
#17226=CARTESIAN_POINT('Origin',(100.910000144262,20.3600005800758,380.));
#17227=CARTESIAN_POINT('',(101.109999564186,20.2600003810484,380.));
#17228=CARTESIAN_POINT('',(101.109999564186,20.3600005800758,380.));
#17229=CARTESIAN_POINT('',(101.309999945234,20.0599999999999,380.));
#17230=CARTESIAN_POINT('Origin',(101.309999945234,20.2600003810484,380.));
#17231=CARTESIAN_POINT('',(109.560000346242,20.0599999999999,380.));
#17232=CARTESIAN_POINT('',(101.309999945234,20.0599999999999,380.));
#17233=CARTESIAN_POINT('',(111.56,22.0599996537577,380.));
#17234=CARTESIAN_POINT('Origin',(109.560000346242,22.0599996537577,380.));
#17235=CARTESIAN_POINT('',(111.56,30.3100004787476,380.));
#17236=CARTESIAN_POINT('',(111.56,22.0599996537577,380.));
#17237=CARTESIAN_POINT('',(111.359999715809,30.5100007629388,380.));
#17238=CARTESIAN_POINT('Origin',(111.359999715809,30.3100004787476,380.));
#17239=CARTESIAN_POINT('',(111.260000611316,30.5100007629388,380.));
#17240=CARTESIAN_POINT('',(111.359999715809,30.5100007629388,380.));
#17241=CARTESIAN_POINT('',(111.060000327124,30.71000104713,380.));
#17242=CARTESIAN_POINT('Origin',(111.260000611316,30.71000104713,380.));
#17243=CARTESIAN_POINT('',(111.060000327124,30.8100004787487,380.));
#17244=CARTESIAN_POINT('',(111.060000327124,30.71000104713,380.));
#17245=CARTESIAN_POINT('',(110.860000042933,31.0100007629399,380.));
#17246=CARTESIAN_POINT('Origin',(110.860000042933,30.8100004787487,380.));
#17247=CARTESIAN_POINT('',(109.959999939919,31.0100007629399,380.));
#17248=CARTESIAN_POINT('',(110.860000042933,31.0100007629399,380.));
#17249=CARTESIAN_POINT('',(109.359999564184,30.4100003872052,380.));
#17250=CARTESIAN_POINT('Origin',(109.959999939919,30.4100003872052,380.));
#17251=CARTESIAN_POINT('',(109.359999564184,27.0100002841911,380.));
#17252=CARTESIAN_POINT('',(109.359999564184,30.4100003872052,380.));
#17253=CARTESIAN_POINT('',(109.159999279993,26.8099999999999,380.));
#17254=CARTESIAN_POINT('Origin',(109.159999279993,27.0100002841911,380.));
#17255=CARTESIAN_POINT('',(106.609999564184,26.8099999999999,380.));
#17256=CARTESIAN_POINT('',(109.159999279993,26.8099999999999,380.));
#17257=CARTESIAN_POINT('',(102.564465430273,30.8555341339111,380.));
#17258=CARTESIAN_POINT('',(106.609999564184,26.8099999999999,380.));
#17259=CARTESIAN_POINT('',(102.564465430273,34.1600003814696,380.));
#17260=CARTESIAN_POINT('',(102.564465430273,30.8555341339111,380.));
#17261=CARTESIAN_POINT('',(102.044852164282,35.0599999999999,380.));
#17262=CARTESIAN_POINT('',(102.564465430273,34.1600003814696,380.));
#17263=CARTESIAN_POINT('',(102.564465430273,35.9599996185302,380.));
#17264=CARTESIAN_POINT('',(102.044852164282,35.0599999999999,380.));
#17265=CARTESIAN_POINT('',(102.564465430273,39.2644658660888,380.));
#17266=CARTESIAN_POINT('',(102.564465430273,35.9599996185302,380.));
#17267=CARTESIAN_POINT('',(106.609999564184,43.3099999999999,380.));
#17268=CARTESIAN_POINT('',(102.564465430273,39.2644658660888,380.));
#17269=CARTESIAN_POINT('',(109.159999279993,43.3099999999999,380.));
#17270=CARTESIAN_POINT('',(106.609999564184,43.3099999999999,380.));
#17271=CARTESIAN_POINT('',(109.359999564184,43.1099997158087,380.));
#17272=CARTESIAN_POINT('Origin',(109.159999279993,43.1099997158087,380.));
#17273=CARTESIAN_POINT('',(109.359999564184,39.7099996127947,380.));
#17274=CARTESIAN_POINT('',(109.359999564184,43.1099997158087,380.));
#17275=CARTESIAN_POINT('',(109.959999939919,39.1099992370599,380.));
#17276=CARTESIAN_POINT('Origin',(109.959999939919,39.7099996127947,380.));
#17277=CARTESIAN_POINT('',(110.860000042933,39.1099992370599,380.));
#17278=CARTESIAN_POINT('',(109.959999939919,39.1099992370599,380.));
#17279=CARTESIAN_POINT('',(111.060000327124,39.3099995212511,380.));
#17280=CARTESIAN_POINT('Origin',(110.860000042933,39.3099995212511,380.));
#17281=CARTESIAN_POINT('',(111.060000327124,39.4099989528698,380.));
#17282=CARTESIAN_POINT('',(111.060000327124,39.3099995212511,380.));
#17283=CARTESIAN_POINT('',(111.260000611316,39.609999237061,380.));
#17284=CARTESIAN_POINT('Origin',(111.260000611316,39.4099989528698,380.));
#17285=CARTESIAN_POINT('',(111.359999715809,39.609999237061,380.));
#17286=CARTESIAN_POINT('',(111.260000611316,39.609999237061,380.));
#17287=CARTESIAN_POINT('',(111.56,39.8099995212523,380.));
#17288=CARTESIAN_POINT('Origin',(111.359999715809,39.8099995212523,380.));
#17289=CARTESIAN_POINT('',(111.56,48.0600003462421,380.));
#17290=CARTESIAN_POINT('',(111.56,39.8099995212523,380.));
#17291=CARTESIAN_POINT('',(109.560000346242,50.0599999999999,380.));
#17292=CARTESIAN_POINT('Origin',(109.560000346242,48.0600003462421,380.));
#17293=CARTESIAN_POINT('',(101.309999945234,50.0599999999999,380.));
#17294=CARTESIAN_POINT('',(109.560000346242,50.0599999999999,380.));
#17295=CARTESIAN_POINT('',(101.109999564186,49.8599996189514,380.));
#17296=CARTESIAN_POINT('Origin',(101.309999945234,49.8599996189514,380.));
#17297=CARTESIAN_POINT('',(101.109999564186,49.759999419924,380.));
#17298=CARTESIAN_POINT('',(101.109999564186,49.8599996189514,380.));
#17299=CARTESIAN_POINT('',(100.910000144262,49.5599999999999,380.));
#17300=CARTESIAN_POINT('Origin',(100.910000144262,49.759999419924,380.));
#17301=CARTESIAN_POINT('',(100.810000373598,49.5599999999999,380.));
#17302=CARTESIAN_POINT('',(100.910000144262,49.5599999999999,380.));
#17303=CARTESIAN_POINT('',(100.61,49.3599996264019,380.));
#17304=CARTESIAN_POINT('Origin',(100.810000373598,49.3599996264019,380.));
#17305=CARTESIAN_POINT('',(100.61,48.4599994339809,380.));
#17306=CARTESIAN_POINT('',(100.61,49.3599996264019,380.));
#17307=CARTESIAN_POINT('',(101.210000196921,47.85999923706,380.));
#17308=CARTESIAN_POINT('Origin',(101.210000196921,48.4599994339809,380.));
#17309=CARTESIAN_POINT('',(104.609999923724,47.85999923706,380.));
#17310=CARTESIAN_POINT('',(101.210000196921,47.85999923706,380.));
#17311=CARTESIAN_POINT('',(104.810000327124,47.6599988336597,380.));
#17312=CARTESIAN_POINT('Origin',(104.609999923724,47.6599988336597,380.));
#17313=CARTESIAN_POINT('',(104.810000327124,45.1099992370597,380.));
#17314=CARTESIAN_POINT('',(104.810000327124,47.6599988336597,380.));
#17315=CARTESIAN_POINT('',(100.764466193213,41.0599999999999,380.));
#17316=CARTESIAN_POINT('',(104.810000327124,45.1099992370597,380.));
#17317=CARTESIAN_POINT('',(97.4599999456547,41.0599999999999,380.));
#17318=CARTESIAN_POINT('',(100.764466193213,41.0599999999999,380.));
#17319=CARTESIAN_POINT('',(96.5599999999999,40.5448518371574,380.));
#17320=CARTESIAN_POINT('',(97.4599999456547,41.0599999999999,380.));
#17321=CARTESIAN_POINT('',(95.6600000543452,41.0599999999999,380.));
#17322=CARTESIAN_POINT('',(96.5599999999999,40.5448518371574,380.));
#17323=CARTESIAN_POINT('',(92.3555338067866,41.0599999999999,380.));
#17324=CARTESIAN_POINT('',(95.6600000543452,41.0599999999999,380.));
#17325=CARTESIAN_POINT('',(88.3099996728755,45.1099992370597,380.));
#17326=CARTESIAN_POINT('',(92.3555338067866,41.0599999999999,380.));
#17327=CARTESIAN_POINT('',(88.3099996728755,47.6599988336597,380.));
#17328=CARTESIAN_POINT('',(88.3099996728755,45.1099992370597,380.));
#17329=CARTESIAN_POINT('',(88.5100000762757,47.85999923706,380.));
#17330=CARTESIAN_POINT('Origin',(88.5100000762757,47.6599988336597,380.));
#17331=CARTESIAN_POINT('',(91.9099998030791,47.85999923706,380.));
#17332=CARTESIAN_POINT('',(88.5100000762757,47.85999923706,380.));
#17333=CARTESIAN_POINT('',(92.5099999999999,48.4599994339809,380.));
#17334=CARTESIAN_POINT('Origin',(91.9099998030791,48.4599994339809,380.));
#17335=CARTESIAN_POINT('',(92.5099999999999,49.3599996264019,380.));
#17336=CARTESIAN_POINT('',(92.5099999999999,48.4599994339809,380.));
#17337=CARTESIAN_POINT('',(92.309999626402,49.5599999999999,380.));
#17338=CARTESIAN_POINT('Origin',(92.309999626402,49.3599996264019,380.));
#17339=CARTESIAN_POINT('',(92.2099998557381,49.5599999999999,380.));
#17340=CARTESIAN_POINT('',(92.309999626402,49.5599999999999,380.));
#17341=CARTESIAN_POINT('',(92.010000435814,49.759999419924,380.));
#17342=CARTESIAN_POINT('Origin',(92.2099998557381,49.759999419924,380.));
#17343=CARTESIAN_POINT('',(92.010000435814,49.8599996189514,380.));
#17344=CARTESIAN_POINT('',(92.010000435814,49.759999419924,380.));
#17345=CARTESIAN_POINT('',(91.8100000547655,50.0599999999999,380.));
#17346=CARTESIAN_POINT('Origin',(91.8100000547655,49.8599996189514,380.));
#17347=CARTESIAN_POINT('',(83.5599996537577,50.0599999999999,380.));
#17348=CARTESIAN_POINT('',(91.8100000547655,50.0599999999999,380.));
#17349=CARTESIAN_POINT('',(81.5599999999999,48.0600003462421,380.));
#17350=CARTESIAN_POINT('Origin',(83.5599996537577,48.0600003462421,380.));
#17351=CARTESIAN_POINT('',(81.5599999999999,39.8099995212522,380.));
#17352=CARTESIAN_POINT('',(81.5599999999999,48.0600003462421,380.));
#17353=CARTESIAN_POINT('',(81.7600002841911,39.609999237061,380.));
#17354=CARTESIAN_POINT('Origin',(81.7600002841911,39.8099995212522,380.));
#17355=CARTESIAN_POINT('',(81.8599993886842,39.609999237061,380.));
#17356=CARTESIAN_POINT('',(81.7600002841911,39.609999237061,380.));
#17357=CARTESIAN_POINT('',(82.0599996728754,39.4099989528698,380.));
#17358=CARTESIAN_POINT('Origin',(81.8599993886842,39.4099989528698,380.));
#17359=CARTESIAN_POINT('',(82.0599996728754,39.3099995212511,380.));
#17360=CARTESIAN_POINT('',(82.0599996728754,39.4099989528698,380.));
#17361=CARTESIAN_POINT('',(82.2599999570666,39.1099992370599,380.));
#17362=CARTESIAN_POINT('Origin',(82.2599999570666,39.3099995212511,380.));
#17363=CARTESIAN_POINT('',(83.1600000600806,39.1099992370599,380.));
#17364=CARTESIAN_POINT('',(82.2599999570666,39.1099992370599,380.));
#17365=CARTESIAN_POINT('',(83.7600004358154,39.7099996127947,380.));
#17366=CARTESIAN_POINT('Origin',(83.1600000600806,39.7099996127947,380.));
#17367=CARTESIAN_POINT('',(83.7600004358154,43.1099997158087,380.));
#17368=CARTESIAN_POINT('',(83.7600004358154,39.7099996127947,380.));
#17369=CARTESIAN_POINT('',(83.9600007200066,43.3099999999999,380.));
#17370=CARTESIAN_POINT('Origin',(83.9600007200066,43.1099997158087,380.));
#17371=CARTESIAN_POINT('',(86.510000435816,43.3099999999999,380.));
#17372=CARTESIAN_POINT('',(83.9600007200066,43.3099999999999,380.));
#17373=CARTESIAN_POINT('',(90.5555345697271,39.2644658660888,380.));
#17374=CARTESIAN_POINT('',(86.510000435816,43.3099999999999,380.));
#17375=CARTESIAN_POINT('',(90.5555345697271,35.9599996185302,380.));
#17376=CARTESIAN_POINT('',(90.5555345697271,39.2644658660888,380.));
#17377=CARTESIAN_POINT('',(91.0751478357183,35.0599999999999,380.));
#17378=CARTESIAN_POINT('',(90.5555345697271,35.9599996185302,380.));
#17379=CARTESIAN_POINT('',(90.5555345697271,34.1600003814696,380.));
#17380=CARTESIAN_POINT('',(91.0751478357183,35.0599999999999,380.));
#17381=CARTESIAN_POINT('',(90.5555345697271,30.8555341339111,380.));
#17382=CARTESIAN_POINT('',(90.5555345697271,34.1600003814696,380.));
#17383=CARTESIAN_POINT('',(86.510000435816,26.8099999999999,380.));
#17384=CARTESIAN_POINT('',(90.5555345697271,30.8555341339111,380.));
#17385=CARTESIAN_POINT('',(83.9600007200066,26.8099999999999,380.));
#17386=CARTESIAN_POINT('',(86.510000435816,26.8099999999999,380.));
#17387=CARTESIAN_POINT('',(83.7600004358154,27.0100002841911,380.));
#17388=CARTESIAN_POINT('Origin',(83.9600007200066,27.0100002841911,380.));
#17389=CARTESIAN_POINT('',(83.7600004358154,30.4100003872052,380.));
#17390=CARTESIAN_POINT('',(83.7600004358154,27.0100002841911,380.));
#17391=CARTESIAN_POINT('',(83.1600000600806,31.0100007629399,380.));
#17392=CARTESIAN_POINT('Origin',(83.1600000600806,30.4100003872052,380.));
#17393=CARTESIAN_POINT('',(82.2599999570666,31.0100007629399,380.));
#17394=CARTESIAN_POINT('',(83.1600000600806,31.0100007629399,380.));
#17395=CARTESIAN_POINT('',(82.0599996728754,30.8100004787487,380.));
#17396=CARTESIAN_POINT('Origin',(82.2599999570666,30.8100004787487,380.));
#17397=CARTESIAN_POINT('',(82.0599996728754,30.71000104713,380.));
#17398=CARTESIAN_POINT('',(82.0599996728754,30.8100004787487,380.));
#17399=CARTESIAN_POINT('',(81.8599993886842,30.5100007629388,380.));
#17400=CARTESIAN_POINT('Origin',(81.8599993886842,30.71000104713,380.));
#17401=CARTESIAN_POINT('',(81.7600002841911,30.5100007629388,380.));
#17402=CARTESIAN_POINT('',(81.8599993886842,30.5100007629388,380.));
#17403=CARTESIAN_POINT('',(81.5599999999999,30.3100004787476,380.));
#17404=CARTESIAN_POINT('Origin',(81.7600002841911,30.3100004787476,380.));
#17405=CARTESIAN_POINT('',(81.5599999999999,22.0599996537577,380.));
#17406=CARTESIAN_POINT('',(81.5599999999999,30.3100004787476,380.));
#17407=CARTESIAN_POINT('',(83.5599996537578,20.0599999999999,380.));
#17408=CARTESIAN_POINT('Origin',(83.5599996537577,22.0599996537577,380.));
#17409=CARTESIAN_POINT('',(91.8100000547655,20.0599999999999,380.));
#17410=CARTESIAN_POINT('',(83.5599996537578,20.0599999999999,380.));
#17411=CARTESIAN_POINT('',(92.010000435814,20.2600003810484,380.));
#17412=CARTESIAN_POINT('Origin',(91.8100000547655,20.2600003810484,380.));
#17413=CARTESIAN_POINT('',(92.010000435814,20.3600005800758,380.));
#17414=CARTESIAN_POINT('',(92.010000435814,20.2600003810484,380.));
#17415=CARTESIAN_POINT('',(92.2099998557381,20.5599999999999,380.));
#17416=CARTESIAN_POINT('Origin',(92.2099998557381,20.3600005800758,380.));
#17417=CARTESIAN_POINT('',(92.309999626402,20.5599999999999,380.));
#17418=CARTESIAN_POINT('',(92.2099998557381,20.5599999999999,380.));
#17419=CARTESIAN_POINT('',(92.5099999999999,20.7600003735979,380.));
#17420=CARTESIAN_POINT('Origin',(92.309999626402,20.7600003735979,380.));
#17421=CARTESIAN_POINT('',(92.5099999999999,21.6600005660189,380.));
#17422=CARTESIAN_POINT('',(92.5099999999999,20.7600003735979,380.));
#17423=CARTESIAN_POINT('',(91.9099998030791,22.2600007629398,380.));
#17424=CARTESIAN_POINT('Origin',(91.9099998030791,21.6600005660189,380.));
#17425=CARTESIAN_POINT('',(88.5100000762757,22.2600007629398,380.));
#17426=CARTESIAN_POINT('',(91.9099998030791,22.2600007629398,380.));
#17427=CARTESIAN_POINT('',(88.3099996728755,22.4600011663401,380.));
#17428=CARTESIAN_POINT('Origin',(88.5100000762757,22.4600011663401,380.));
#17429=CARTESIAN_POINT('',(88.3099996728755,25.0100007629401,380.));
#17430=CARTESIAN_POINT('',(88.3099996728755,22.4600011663401,380.));
#17431=CARTESIAN_POINT('',(92.3555338067866,29.0599999999999,380.));
#17432=CARTESIAN_POINT('',(88.3099996728755,25.0100007629401,380.));
#17433=CARTESIAN_POINT('',(92.3555338067866,29.0599999999999,380.));
#17434=CARTESIAN_POINT('',(109.260001090064,48.7600003984092,380.));
#17435=CARTESIAN_POINT('',(107.060000327124,48.7600003984092,380.));
#17436=CARTESIAN_POINT('',(109.260001090064,48.7600003984092,380.));
#17437=CARTESIAN_POINT('',(110.260001090064,47.7600003984092,380.));
#17438=CARTESIAN_POINT('Origin',(109.260001099622,47.7600004079674,380.));
#17439=CARTESIAN_POINT('',(110.260001090064,45.5599996354697,380.));
#17440=CARTESIAN_POINT('',(110.260001090064,45.5599996354697,380.));
#17441=CARTESIAN_POINT('',(109.260001090064,44.5599996354697,380.));
#17442=CARTESIAN_POINT('Origin',(109.260001099622,45.5599996259115,380.));
#17443=CARTESIAN_POINT('',(107.060000327124,44.5599996354697,380.));
#17444=CARTESIAN_POINT('',(107.060000327124,44.5599996354697,380.));
#17445=CARTESIAN_POINT('',(106.060000327124,45.5599996354697,380.));
#17446=CARTESIAN_POINT('Origin',(107.060000317566,45.5599996259115,380.));
#17447=CARTESIAN_POINT('',(106.060000327124,47.7600003984092,380.));
#17448=CARTESIAN_POINT('',(106.060000327124,47.7600003984092,380.));
#17449=CARTESIAN_POINT('Origin',(107.060000317566,47.7600004079674,380.));
#17450=CARTESIAN_POINT('',(94.9598704761907,38.3405617669895,380.));
#17451=CARTESIAN_POINT('',(93.4240705880017,39.5784009033024,380.));
#17452=CARTESIAN_POINT('',(94.9598704761907,38.3405617669895,380.));
#17453=CARTESIAN_POINT('',(98.1601295238092,38.3405617669895,380.));
#17454=CARTESIAN_POINT('Origin',(96.5599999999999,35.0599999999999,380.));
#17455=CARTESIAN_POINT('',(99.6959294119981,39.5784009033024,380.));
#17456=CARTESIAN_POINT('',(99.6959294119981,39.5784009033024,380.));
#17457=CARTESIAN_POINT('',(101.065336892425,38.2146694732975,380.));
#17458=CARTESIAN_POINT('Origin',(96.5599999999999,35.0599999999999,380.));
#17459=CARTESIAN_POINT('',(99.8405617315319,36.6601295965039,380.));
#17460=CARTESIAN_POINT('',(99.8405617315319,36.6601295965039,380.));
#17461=CARTESIAN_POINT('',(99.8405617315319,33.459870403496,380.));
#17462=CARTESIAN_POINT('Origin',(96.5599999999999,35.0599999999999,380.));
#17463=CARTESIAN_POINT('',(101.065336892425,31.9053305267024,380.));
#17464=CARTESIAN_POINT('',(101.065336892425,31.9053305267024,380.));
#17465=CARTESIAN_POINT('',(99.6959294119981,30.5415990966974,380.));
#17466=CARTESIAN_POINT('Origin',(96.5599999999999,35.0599999999999,380.));
#17467=CARTESIAN_POINT('',(98.1601295238092,31.7794382330103,380.));
#17468=CARTESIAN_POINT('',(98.1601295238092,31.7794382330103,380.));
#17469=CARTESIAN_POINT('',(94.9598704761907,31.7794382330103,380.));
#17470=CARTESIAN_POINT('Origin',(96.5599999999999,35.0599999999999,380.));
#17471=CARTESIAN_POINT('',(93.4240705880018,30.5415990966974,380.));
#17472=CARTESIAN_POINT('',(93.4240705880018,30.5415990966974,380.));
#17473=CARTESIAN_POINT('',(92.0546631075751,31.9053305267024,380.));
#17474=CARTESIAN_POINT('Origin',(96.5599999999999,35.0599999999999,380.));
#17475=CARTESIAN_POINT('',(93.279438268468,33.4598704034959,380.));
#17476=CARTESIAN_POINT('',(92.0546631075751,38.2146694732975,380.));
#17477=CARTESIAN_POINT('',(92.0546631075751,38.2146694732975,380.));
#17478=CARTESIAN_POINT('Origin',(96.5599999999999,35.0599999999999,380.));
#17479=CARTESIAN_POINT('',(83.859998909936,21.3599996015906,380.));
#17480=CARTESIAN_POINT('',(86.0599996728755,21.3599996015906,380.));
#17481=CARTESIAN_POINT('',(83.859998909936,21.3599996015906,380.));
#17482=CARTESIAN_POINT('',(82.8599989099361,22.3599996015906,380.));
#17483=CARTESIAN_POINT('Origin',(83.8599989003778,22.3599995920324,380.));
#17484=CARTESIAN_POINT('',(82.859998909936,24.5600003645301,380.));
#17485=CARTESIAN_POINT('',(82.859998909936,24.5600003645301,380.));
#17486=CARTESIAN_POINT('',(83.859998909936,25.5600003645301,380.));
#17487=CARTESIAN_POINT('Origin',(83.8599989003778,24.5600003740883,380.));
#17488=CARTESIAN_POINT('',(86.0599996728755,25.5600003645301,380.));
#17489=CARTESIAN_POINT('',(86.0599996728755,25.5600003645301,380.));
#17490=CARTESIAN_POINT('',(87.0599996728755,24.5600003645301,380.));
#17491=CARTESIAN_POINT('Origin',(86.0599996824337,24.5600003740883,380.));
#17492=CARTESIAN_POINT('',(87.0599996728755,22.3599996015906,380.));
#17493=CARTESIAN_POINT('',(87.0599996728755,22.3599996015906,380.));
#17494=CARTESIAN_POINT('Origin',(86.0599996824337,22.3599995920324,380.));
#17495=CARTESIAN_POINT('',(110.260001090064,22.3599996015906,380.));
#17496=CARTESIAN_POINT('',(110.260001090064,24.5600003645301,380.));
#17497=CARTESIAN_POINT('',(110.260001090064,22.3599996015906,380.));
#17498=CARTESIAN_POINT('',(109.260001090064,21.3599996015906,380.));
#17499=CARTESIAN_POINT('Origin',(109.260001099622,22.3599995920324,380.));
#17500=CARTESIAN_POINT('',(107.060000327124,21.3599996015906,380.));
#17501=CARTESIAN_POINT('',(107.060000327124,21.3599996015906,380.));
#17502=CARTESIAN_POINT('',(106.060000327124,22.3599996015906,380.));
#17503=CARTESIAN_POINT('Origin',(107.060000317566,22.3599995920324,380.));
#17504=CARTESIAN_POINT('',(106.060000327124,24.5600003645301,380.));
#17505=CARTESIAN_POINT('',(106.060000327124,24.5600003645301,380.));
#17506=CARTESIAN_POINT('',(107.060000327124,25.5600003645301,380.));
#17507=CARTESIAN_POINT('Origin',(107.060000317566,24.5600003740883,380.));
#17508=CARTESIAN_POINT('',(109.260001090064,25.5600003645301,380.));
#17509=CARTESIAN_POINT('',(109.260001090064,25.5600003645301,380.));
#17510=CARTESIAN_POINT('Origin',(109.260001099622,24.5600003740883,380.));
#17511=CARTESIAN_POINT('',(86.0599996728755,48.7600003984092,380.));
#17512=CARTESIAN_POINT('',(83.859998909936,48.7600003984092,380.));
#17513=CARTESIAN_POINT('',(86.0599996728755,48.7600003984092,380.));
#17514=CARTESIAN_POINT('',(87.0599996728755,47.7600003984092,380.));
#17515=CARTESIAN_POINT('Origin',(86.0599996824337,47.7600004079674,380.));
#17516=CARTESIAN_POINT('',(87.0599996728755,45.5599996354697,380.));
#17517=CARTESIAN_POINT('',(87.0599996728755,45.5599996354697,380.));
#17518=CARTESIAN_POINT('',(86.0599996728755,44.5599996354697,380.));
#17519=CARTESIAN_POINT('Origin',(86.0599996824337,45.5599996259115,380.));
#17520=CARTESIAN_POINT('',(83.8599989099361,44.5599996354697,380.));
#17521=CARTESIAN_POINT('',(83.8599989099361,44.5599996354697,380.));
#17522=CARTESIAN_POINT('',(82.8599989099361,45.5599996354697,380.));
#17523=CARTESIAN_POINT('Origin',(83.8599989003778,45.5599996259115,380.));
#17524=CARTESIAN_POINT('',(82.8599989099361,47.7600003984092,380.));
#17525=CARTESIAN_POINT('',(82.859998909936,47.7600003984092,380.));
#17526=CARTESIAN_POINT('Origin',(83.8599989003778,47.7600004079674,380.));
#17527=CARTESIAN_POINT('Origin',(104.609999923724,22.4600011663401,0.));
#17528=CARTESIAN_POINT('',(95.6600000543452,29.0599999999999,0.));
#17529=CARTESIAN_POINT('',(96.5599999999999,29.5751481628425,0.));
#17530=CARTESIAN_POINT('',(95.6600000543452,29.0599999999999,0.));
#17531=CARTESIAN_POINT('',(92.3555338067866,29.0599999999999,0.));
#17532=CARTESIAN_POINT('',(92.3555338067866,29.0599999999999,0.));
#17533=CARTESIAN_POINT('',(88.3099996728755,25.0100007629401,0.));
#17534=CARTESIAN_POINT('',(88.3099996728755,25.0100007629401,0.));
#17535=CARTESIAN_POINT('',(88.3099996728755,22.4600011663401,0.));
#17536=CARTESIAN_POINT('',(88.3099996728755,22.4600011663401,0.));
#17537=CARTESIAN_POINT('',(88.5100000762757,22.2600007629398,0.));
#17538=CARTESIAN_POINT('Origin',(88.5100000762757,22.4600011663401,0.));
#17539=CARTESIAN_POINT('',(91.9099998030791,22.2600007629398,0.));
#17540=CARTESIAN_POINT('',(91.9099998030791,22.2600007629398,0.));
#17541=CARTESIAN_POINT('',(92.5099999999999,21.6600005660189,0.));
#17542=CARTESIAN_POINT('Origin',(91.9099998030791,21.6600005660189,0.));
#17543=CARTESIAN_POINT('',(92.5099999999999,20.7600003735979,0.));
#17544=CARTESIAN_POINT('',(92.5099999999999,20.7600003735979,0.));
#17545=CARTESIAN_POINT('',(92.309999626402,20.5599999999999,0.));
#17546=CARTESIAN_POINT('Origin',(92.309999626402,20.7600003735979,0.));
#17547=CARTESIAN_POINT('',(92.2099998557381,20.5599999999999,0.));
#17548=CARTESIAN_POINT('',(92.2099998557381,20.5599999999999,0.));
#17549=CARTESIAN_POINT('',(92.010000435814,20.3600005800758,0.));
#17550=CARTESIAN_POINT('Origin',(92.2099998557381,20.3600005800758,0.));
#17551=CARTESIAN_POINT('',(92.010000435814,20.2600003810484,0.));
#17552=CARTESIAN_POINT('',(92.010000435814,20.2600003810484,0.));
#17553=CARTESIAN_POINT('',(91.8100000547655,20.0599999999999,0.));
#17554=CARTESIAN_POINT('Origin',(91.8100000547655,20.2600003810484,0.));
#17555=CARTESIAN_POINT('',(83.5599996537578,20.0599999999999,0.));
#17556=CARTESIAN_POINT('',(83.5599996537578,20.0599999999999,0.));
#17557=CARTESIAN_POINT('',(81.5599999999999,22.0599996537577,0.));
#17558=CARTESIAN_POINT('Origin',(83.5599996537577,22.0599996537577,0.));
#17559=CARTESIAN_POINT('',(81.5599999999999,30.3100004787476,0.));
#17560=CARTESIAN_POINT('',(81.5599999999999,30.3100004787476,0.));
#17561=CARTESIAN_POINT('',(81.7600002841911,30.5100007629388,0.));
#17562=CARTESIAN_POINT('Origin',(81.7600002841911,30.3100004787476,0.));
#17563=CARTESIAN_POINT('',(81.8599993886842,30.5100007629388,0.));
#17564=CARTESIAN_POINT('',(81.8599993886842,30.5100007629388,0.));
#17565=CARTESIAN_POINT('',(82.0599996728754,30.71000104713,0.));
#17566=CARTESIAN_POINT('Origin',(81.8599993886842,30.71000104713,0.));
#17567=CARTESIAN_POINT('',(82.0599996728754,30.8100004787487,0.));
#17568=CARTESIAN_POINT('',(82.0599996728754,30.8100004787487,0.));
#17569=CARTESIAN_POINT('',(82.2599999570666,31.0100007629399,0.));
#17570=CARTESIAN_POINT('Origin',(82.2599999570666,30.8100004787487,0.));
#17571=CARTESIAN_POINT('',(83.1600000600806,31.0100007629399,0.));
#17572=CARTESIAN_POINT('',(83.1600000600806,31.0100007629399,0.));
#17573=CARTESIAN_POINT('',(83.7600004358154,30.4100003872052,0.));
#17574=CARTESIAN_POINT('Origin',(83.1600000600806,30.4100003872052,0.));
#17575=CARTESIAN_POINT('',(83.7600004358154,27.0100002841911,0.));
#17576=CARTESIAN_POINT('',(83.7600004358154,27.0100002841911,0.));
#17577=CARTESIAN_POINT('',(83.9600007200066,26.8099999999999,0.));
#17578=CARTESIAN_POINT('Origin',(83.9600007200066,27.0100002841911,0.));
#17579=CARTESIAN_POINT('',(86.510000435816,26.8099999999999,0.));
#17580=CARTESIAN_POINT('',(86.510000435816,26.8099999999999,0.));
#17581=CARTESIAN_POINT('',(90.5555345697271,30.8555341339111,0.));
#17582=CARTESIAN_POINT('',(90.5555345697271,30.8555341339111,0.));
#17583=CARTESIAN_POINT('',(90.5555345697271,34.1600003814696,0.));
#17584=CARTESIAN_POINT('',(90.5555345697271,34.1600003814696,0.));
#17585=CARTESIAN_POINT('',(91.0751478357183,35.0599999999999,0.));
#17586=CARTESIAN_POINT('',(91.0751478357183,35.0599999999999,0.));
#17587=CARTESIAN_POINT('',(90.5555345697271,35.9599996185302,0.));
#17588=CARTESIAN_POINT('',(90.5555345697271,35.9599996185302,0.));
#17589=CARTESIAN_POINT('',(90.5555345697271,39.2644658660888,0.));
#17590=CARTESIAN_POINT('',(90.5555345697271,39.2644658660888,0.));
#17591=CARTESIAN_POINT('',(86.510000435816,43.3099999999999,0.));
#17592=CARTESIAN_POINT('',(86.510000435816,43.3099999999999,0.));
#17593=CARTESIAN_POINT('',(83.9600007200066,43.3099999999999,0.));
#17594=CARTESIAN_POINT('',(83.9600007200066,43.3099999999999,0.));
#17595=CARTESIAN_POINT('',(83.7600004358154,43.1099997158087,0.));
#17596=CARTESIAN_POINT('Origin',(83.9600007200066,43.1099997158087,0.));
#17597=CARTESIAN_POINT('',(83.7600004358154,39.7099996127947,0.));
#17598=CARTESIAN_POINT('',(83.7600004358154,39.7099996127947,0.));
#17599=CARTESIAN_POINT('',(83.1600000600806,39.1099992370599,0.));
#17600=CARTESIAN_POINT('Origin',(83.1600000600806,39.7099996127947,0.));
#17601=CARTESIAN_POINT('',(82.2599999570666,39.1099992370599,0.));
#17602=CARTESIAN_POINT('',(82.2599999570666,39.1099992370599,0.));
#17603=CARTESIAN_POINT('',(82.0599996728754,39.3099995212511,0.));
#17604=CARTESIAN_POINT('Origin',(82.2599999570666,39.3099995212511,0.));
#17605=CARTESIAN_POINT('',(82.0599996728754,39.4099989528698,0.));
#17606=CARTESIAN_POINT('',(82.0599996728754,39.4099989528698,0.));
#17607=CARTESIAN_POINT('',(81.8599993886842,39.609999237061,0.));
#17608=CARTESIAN_POINT('Origin',(81.8599993886842,39.4099989528698,0.));
#17609=CARTESIAN_POINT('',(81.7600002841911,39.609999237061,0.));
#17610=CARTESIAN_POINT('',(81.7600002841911,39.609999237061,0.));
#17611=CARTESIAN_POINT('',(81.5599999999999,39.8099995212522,0.));
#17612=CARTESIAN_POINT('Origin',(81.7600002841911,39.8099995212522,0.));
#17613=CARTESIAN_POINT('',(81.5599999999999,48.0600003462421,0.));
#17614=CARTESIAN_POINT('',(81.5599999999999,48.0600003462421,0.));
#17615=CARTESIAN_POINT('',(83.5599996537577,50.0599999999999,0.));
#17616=CARTESIAN_POINT('Origin',(83.5599996537577,48.0600003462421,0.));
#17617=CARTESIAN_POINT('',(91.8100000547655,50.0599999999999,0.));
#17618=CARTESIAN_POINT('',(91.8100000547655,50.0599999999999,0.));
#17619=CARTESIAN_POINT('',(92.010000435814,49.8599996189514,0.));
#17620=CARTESIAN_POINT('Origin',(91.8100000547655,49.8599996189514,0.));
#17621=CARTESIAN_POINT('',(92.010000435814,49.759999419924,0.));
#17622=CARTESIAN_POINT('',(92.010000435814,49.759999419924,0.));
#17623=CARTESIAN_POINT('',(92.2099998557381,49.5599999999999,0.));
#17624=CARTESIAN_POINT('Origin',(92.2099998557381,49.759999419924,0.));
#17625=CARTESIAN_POINT('',(92.309999626402,49.5599999999999,0.));
#17626=CARTESIAN_POINT('',(92.309999626402,49.5599999999999,0.));
#17627=CARTESIAN_POINT('',(92.5099999999999,49.3599996264019,0.));
#17628=CARTESIAN_POINT('Origin',(92.309999626402,49.3599996264019,0.));
#17629=CARTESIAN_POINT('',(92.5099999999999,48.4599994339809,0.));
#17630=CARTESIAN_POINT('',(92.5099999999999,48.4599994339809,0.));
#17631=CARTESIAN_POINT('',(91.9099998030791,47.85999923706,0.));
#17632=CARTESIAN_POINT('Origin',(91.9099998030791,48.4599994339809,0.));
#17633=CARTESIAN_POINT('',(88.5100000762757,47.85999923706,0.));
#17634=CARTESIAN_POINT('',(88.5100000762757,47.85999923706,0.));
#17635=CARTESIAN_POINT('',(88.3099996728755,47.6599988336597,0.));
#17636=CARTESIAN_POINT('Origin',(88.5100000762757,47.6599988336597,0.));
#17637=CARTESIAN_POINT('',(88.3099996728755,45.1099992370597,0.));
#17638=CARTESIAN_POINT('',(88.3099996728755,45.1099992370597,0.));
#17639=CARTESIAN_POINT('',(92.3555338067866,41.0599999999999,0.));
#17640=CARTESIAN_POINT('',(92.3555338067866,41.0599999999999,0.));
#17641=CARTESIAN_POINT('',(95.6600000543452,41.0599999999999,0.));
#17642=CARTESIAN_POINT('',(95.6600000543452,41.0599999999999,0.));
#17643=CARTESIAN_POINT('',(96.5599999999999,40.5448518371574,0.));
#17644=CARTESIAN_POINT('',(96.5599999999999,40.5448518371574,0.));
#17645=CARTESIAN_POINT('',(97.4599999456547,41.0599999999999,0.));
#17646=CARTESIAN_POINT('',(97.4599999456547,41.0599999999999,0.));
#17647=CARTESIAN_POINT('',(100.764466193213,41.0599999999999,0.));
#17648=CARTESIAN_POINT('',(100.764466193213,41.0599999999999,0.));
#17649=CARTESIAN_POINT('',(104.810000327124,45.1099992370597,0.));
#17650=CARTESIAN_POINT('',(104.810000327124,45.1099992370597,0.));
#17651=CARTESIAN_POINT('',(104.810000327124,47.6599988336597,0.));
#17652=CARTESIAN_POINT('',(104.810000327124,47.6599988336597,0.));
#17653=CARTESIAN_POINT('',(104.609999923724,47.85999923706,0.));
#17654=CARTESIAN_POINT('Origin',(104.609999923724,47.6599988336597,0.));
#17655=CARTESIAN_POINT('',(101.210000196921,47.85999923706,0.));
#17656=CARTESIAN_POINT('',(101.210000196921,47.85999923706,0.));
#17657=CARTESIAN_POINT('',(100.61,48.4599994339809,0.));
#17658=CARTESIAN_POINT('Origin',(101.210000196921,48.4599994339809,0.));
#17659=CARTESIAN_POINT('',(100.61,49.3599996264019,0.));
#17660=CARTESIAN_POINT('',(100.61,49.3599996264019,0.));
#17661=CARTESIAN_POINT('',(100.810000373598,49.5599999999999,0.));
#17662=CARTESIAN_POINT('Origin',(100.810000373598,49.3599996264019,0.));
#17663=CARTESIAN_POINT('',(100.910000144262,49.5599999999999,0.));
#17664=CARTESIAN_POINT('',(100.910000144262,49.5599999999999,0.));
#17665=CARTESIAN_POINT('',(101.109999564186,49.759999419924,0.));
#17666=CARTESIAN_POINT('Origin',(100.910000144262,49.759999419924,0.));
#17667=CARTESIAN_POINT('',(101.109999564186,49.8599996189514,0.));
#17668=CARTESIAN_POINT('',(101.109999564186,49.8599996189514,0.));
#17669=CARTESIAN_POINT('',(101.309999945234,50.0599999999999,0.));
#17670=CARTESIAN_POINT('Origin',(101.309999945234,49.8599996189514,0.));
#17671=CARTESIAN_POINT('',(109.560000346242,50.0599999999999,0.));
#17672=CARTESIAN_POINT('',(109.560000346242,50.0599999999999,0.));
#17673=CARTESIAN_POINT('',(111.56,48.0600003462421,0.));
#17674=CARTESIAN_POINT('Origin',(109.560000346242,48.0600003462421,0.));
#17675=CARTESIAN_POINT('',(111.56,39.8099995212523,0.));
#17676=CARTESIAN_POINT('',(111.56,39.8099995212523,0.));
#17677=CARTESIAN_POINT('',(111.359999715809,39.609999237061,0.));
#17678=CARTESIAN_POINT('Origin',(111.359999715809,39.8099995212523,0.));
#17679=CARTESIAN_POINT('',(111.260000611316,39.609999237061,0.));
#17680=CARTESIAN_POINT('',(111.260000611316,39.609999237061,0.));
#17681=CARTESIAN_POINT('',(111.060000327124,39.4099989528698,0.));
#17682=CARTESIAN_POINT('Origin',(111.260000611316,39.4099989528698,0.));
#17683=CARTESIAN_POINT('',(111.060000327124,39.3099995212511,0.));
#17684=CARTESIAN_POINT('',(111.060000327124,39.3099995212511,0.));
#17685=CARTESIAN_POINT('',(110.860000042933,39.1099992370599,0.));
#17686=CARTESIAN_POINT('Origin',(110.860000042933,39.3099995212511,0.));
#17687=CARTESIAN_POINT('',(109.959999939919,39.1099992370599,0.));
#17688=CARTESIAN_POINT('',(109.959999939919,39.1099992370599,0.));
#17689=CARTESIAN_POINT('',(109.359999564184,39.7099996127947,0.));
#17690=CARTESIAN_POINT('Origin',(109.959999939919,39.7099996127947,0.));
#17691=CARTESIAN_POINT('',(109.359999564184,43.1099997158087,0.));
#17692=CARTESIAN_POINT('',(109.359999564184,43.1099997158087,0.));
#17693=CARTESIAN_POINT('',(109.159999279993,43.3099999999999,0.));
#17694=CARTESIAN_POINT('Origin',(109.159999279993,43.1099997158087,0.));
#17695=CARTESIAN_POINT('',(106.609999564184,43.3099999999999,0.));
#17696=CARTESIAN_POINT('',(106.609999564184,43.3099999999999,0.));
#17697=CARTESIAN_POINT('',(102.564465430273,39.2644658660888,0.));
#17698=CARTESIAN_POINT('',(102.564465430273,39.2644658660888,0.));
#17699=CARTESIAN_POINT('',(102.564465430273,35.9599996185302,0.));
#17700=CARTESIAN_POINT('',(102.564465430273,35.9599996185302,0.));
#17701=CARTESIAN_POINT('',(102.044852164282,35.0599999999999,0.));
#17702=CARTESIAN_POINT('',(102.044852164282,35.0599999999999,0.));
#17703=CARTESIAN_POINT('',(102.564465430273,34.1600003814696,0.));
#17704=CARTESIAN_POINT('',(102.564465430273,34.1600003814696,0.));
#17705=CARTESIAN_POINT('',(102.564465430273,30.8555341339111,0.));
#17706=CARTESIAN_POINT('',(102.564465430273,30.8555341339111,0.));
#17707=CARTESIAN_POINT('',(106.609999564184,26.8099999999999,0.));
#17708=CARTESIAN_POINT('',(106.609999564184,26.8099999999999,0.));
#17709=CARTESIAN_POINT('',(109.159999279993,26.8099999999999,0.));
#17710=CARTESIAN_POINT('',(109.159999279993,26.8099999999999,0.));
#17711=CARTESIAN_POINT('',(109.359999564184,27.0100002841911,0.));
#17712=CARTESIAN_POINT('Origin',(109.159999279993,27.0100002841911,0.));
#17713=CARTESIAN_POINT('',(109.359999564184,30.4100003872052,0.));
#17714=CARTESIAN_POINT('',(109.359999564184,30.4100003872052,0.));
#17715=CARTESIAN_POINT('',(109.959999939919,31.0100007629399,0.));
#17716=CARTESIAN_POINT('Origin',(109.959999939919,30.4100003872052,0.));
#17717=CARTESIAN_POINT('',(110.860000042933,31.0100007629399,0.));
#17718=CARTESIAN_POINT('',(110.860000042933,31.0100007629399,0.));
#17719=CARTESIAN_POINT('',(111.060000327124,30.8100004787487,0.));
#17720=CARTESIAN_POINT('Origin',(110.860000042933,30.8100004787487,0.));
#17721=CARTESIAN_POINT('',(111.060000327124,30.71000104713,0.));
#17722=CARTESIAN_POINT('',(111.060000327124,30.71000104713,0.));
#17723=CARTESIAN_POINT('',(111.260000611316,30.5100007629388,0.));
#17724=CARTESIAN_POINT('Origin',(111.260000611316,30.71000104713,0.));
#17725=CARTESIAN_POINT('',(111.359999715809,30.5100007629388,0.));
#17726=CARTESIAN_POINT('',(111.359999715809,30.5100007629388,0.));
#17727=CARTESIAN_POINT('',(111.56,30.3100004787476,0.));
#17728=CARTESIAN_POINT('Origin',(111.359999715809,30.3100004787476,0.));
#17729=CARTESIAN_POINT('',(111.56,22.0599996537577,0.));
#17730=CARTESIAN_POINT('',(111.56,22.0599996537577,0.));
#17731=CARTESIAN_POINT('',(109.560000346242,20.0599999999999,0.));
#17732=CARTESIAN_POINT('Origin',(109.560000346242,22.0599996537577,0.));
#17733=CARTESIAN_POINT('',(101.309999945234,20.0599999999999,0.));
#17734=CARTESIAN_POINT('',(101.309999945234,20.0599999999999,0.));
#17735=CARTESIAN_POINT('',(101.109999564186,20.2600003810484,0.));
#17736=CARTESIAN_POINT('Origin',(101.309999945234,20.2600003810484,0.));
#17737=CARTESIAN_POINT('',(101.109999564186,20.3600005800758,0.));
#17738=CARTESIAN_POINT('',(101.109999564186,20.3600005800758,0.));
#17739=CARTESIAN_POINT('',(100.910000144262,20.5599999999999,0.));
#17740=CARTESIAN_POINT('Origin',(100.910000144262,20.3600005800758,0.));
#17741=CARTESIAN_POINT('',(100.810000373598,20.5599999999999,0.));
#17742=CARTESIAN_POINT('',(100.810000373598,20.5599999999999,0.));
#17743=CARTESIAN_POINT('',(100.61,20.7600003735979,0.));
#17744=CARTESIAN_POINT('Origin',(100.810000373598,20.7600003735979,0.));
#17745=CARTESIAN_POINT('',(100.61,21.6600005660189,0.));
#17746=CARTESIAN_POINT('',(100.61,21.6600005660189,0.));
#17747=CARTESIAN_POINT('',(101.210000196921,22.2600007629398,0.));
#17748=CARTESIAN_POINT('Origin',(101.210000196921,21.6600005660189,0.));
#17749=CARTESIAN_POINT('',(104.609999923724,22.2600007629398,0.));
#17750=CARTESIAN_POINT('',(104.609999923724,22.2600007629398,0.));
#17751=CARTESIAN_POINT('',(104.810000327124,22.4600011663401,0.));
#17752=CARTESIAN_POINT('Origin',(104.609999923724,22.4600011663401,0.));
#17753=CARTESIAN_POINT('',(104.810000327124,25.0100007629401,0.));
#17754=CARTESIAN_POINT('',(104.810000327124,25.0100007629401,0.));
#17755=CARTESIAN_POINT('',(100.764466193213,29.0599999999999,0.));
#17756=CARTESIAN_POINT('',(100.764466193213,29.0599999999999,0.));
#17757=CARTESIAN_POINT('',(97.4599999456547,29.0599999999999,0.));
#17758=CARTESIAN_POINT('',(97.4599999456547,29.0599999999999,0.));
#17759=CARTESIAN_POINT('',(96.5599999999999,29.5751481628425,0.));
#17760=CARTESIAN_POINT('',(110.260001090064,47.7600003984092,0.));
#17761=CARTESIAN_POINT('',(109.260001090064,48.7600003984092,0.));
#17762=CARTESIAN_POINT('Origin',(109.260001099622,47.7600004079674,0.));
#17763=CARTESIAN_POINT('',(107.060000327124,48.7600003984092,0.));
#17764=CARTESIAN_POINT('',(109.260001090064,48.7600003984092,0.));
#17765=CARTESIAN_POINT('',(106.060000327124,47.7600003984092,0.));
#17766=CARTESIAN_POINT('Origin',(107.060000317566,47.7600004079674,0.));
#17767=CARTESIAN_POINT('',(106.060000327124,45.5599996354697,0.));
#17768=CARTESIAN_POINT('',(106.060000327124,47.7600003984092,0.));
#17769=CARTESIAN_POINT('',(107.060000327124,44.5599996354697,0.));
#17770=CARTESIAN_POINT('Origin',(107.060000317566,45.5599996259115,0.));
#17771=CARTESIAN_POINT('',(109.260001090064,44.5599996354697,0.));
#17772=CARTESIAN_POINT('',(107.060000327124,44.5599996354697,0.));
#17773=CARTESIAN_POINT('',(110.260001090064,45.5599996354697,0.));
#17774=CARTESIAN_POINT('Origin',(109.260001099622,45.5599996259115,0.));
#17775=CARTESIAN_POINT('',(110.260001090064,45.5599996354697,0.));
#17776=CARTESIAN_POINT('',(82.8599989099361,22.3599996015906,0.));
#17777=CARTESIAN_POINT('',(83.859998909936,21.3599996015906,0.));
#17778=CARTESIAN_POINT('Origin',(83.8599989003778,22.3599995920324,0.));
#17779=CARTESIAN_POINT('',(86.0599996728755,21.3599996015906,0.));
#17780=CARTESIAN_POINT('',(83.859998909936,21.3599996015906,0.));
#17781=CARTESIAN_POINT('',(87.0599996728755,22.3599996015906,0.));
#17782=CARTESIAN_POINT('Origin',(86.0599996824337,22.3599995920324,0.));
#17783=CARTESIAN_POINT('',(87.0599996728755,24.5600003645301,0.));
#17784=CARTESIAN_POINT('',(87.0599996728755,22.3599996015906,0.));
#17785=CARTESIAN_POINT('',(86.0599996728755,25.5600003645301,0.));
#17786=CARTESIAN_POINT('Origin',(86.0599996824337,24.5600003740883,0.));
#17787=CARTESIAN_POINT('',(83.859998909936,25.5600003645301,0.));
#17788=CARTESIAN_POINT('',(86.0599996728755,25.5600003645301,0.));
#17789=CARTESIAN_POINT('',(82.8599989099361,24.5600003645301,0.));
#17790=CARTESIAN_POINT('Origin',(83.8599989003778,24.5600003740883,0.));
#17791=CARTESIAN_POINT('',(82.859998909936,24.5600003645301,0.));
#17792=CARTESIAN_POINT('',(87.0599996728755,47.7600003984092,0.));
#17793=CARTESIAN_POINT('',(86.0599996728755,48.7600003984092,0.));
#17794=CARTESIAN_POINT('Origin',(86.0599996824337,47.7600004079674,0.));
#17795=CARTESIAN_POINT('',(83.859998909936,48.7600003984092,0.));
#17796=CARTESIAN_POINT('',(86.0599996728755,48.7600003984092,0.));
#17797=CARTESIAN_POINT('',(82.8599989099361,47.7600003984092,0.));
#17798=CARTESIAN_POINT('Origin',(83.8599989003778,47.7600004079674,0.));
#17799=CARTESIAN_POINT('',(82.8599989099361,45.5599996354697,0.));
#17800=CARTESIAN_POINT('',(82.859998909936,47.7600003984092,0.));
#17801=CARTESIAN_POINT('',(83.8599989099361,44.5599996354697,0.));
#17802=CARTESIAN_POINT('Origin',(83.8599989003778,45.5599996259115,0.));
#17803=CARTESIAN_POINT('',(86.0599996728755,44.5599996354697,0.));
#17804=CARTESIAN_POINT('',(83.8599989099361,44.5599996354697,0.));
#17805=CARTESIAN_POINT('',(87.0599996728755,45.5599996354697,0.));
#17806=CARTESIAN_POINT('Origin',(86.0599996824337,45.5599996259115,0.));
#17807=CARTESIAN_POINT('',(87.0599996728755,45.5599996354697,0.));
#17808=CARTESIAN_POINT('',(109.260001090064,21.3599996015906,0.));
#17809=CARTESIAN_POINT('',(110.260001090064,22.3599996015906,0.));
#17810=CARTESIAN_POINT('Origin',(109.260001099622,22.3599995920324,0.));
#17811=CARTESIAN_POINT('',(110.260001090064,24.5600003645301,0.));
#17812=CARTESIAN_POINT('',(110.260001090064,22.3599996015906,0.));
#17813=CARTESIAN_POINT('',(109.260001090064,25.5600003645301,0.));
#17814=CARTESIAN_POINT('Origin',(109.260001099622,24.5600003740883,0.));
#17815=CARTESIAN_POINT('',(107.060000327124,25.5600003645301,0.));
#17816=CARTESIAN_POINT('',(109.260001090064,25.5600003645301,0.));
#17817=CARTESIAN_POINT('',(106.060000327124,24.5600003645301,0.));
#17818=CARTESIAN_POINT('Origin',(107.060000317566,24.5600003740883,0.));
#17819=CARTESIAN_POINT('',(106.060000327124,22.3599996015906,0.));
#17820=CARTESIAN_POINT('',(106.060000327124,24.5600003645301,0.));
#17821=CARTESIAN_POINT('',(107.060000327124,21.3599996015906,0.));
#17822=CARTESIAN_POINT('Origin',(107.060000317566,22.3599995920324,0.));
#17823=CARTESIAN_POINT('',(107.060000327124,21.3599996015906,0.));
#17824=CARTESIAN_POINT('',(98.1601295238092,38.3405617669895,0.));
#17825=CARTESIAN_POINT('',(94.9598704761907,38.3405617669895,0.));
#17826=CARTESIAN_POINT('Origin',(96.5599999999999,35.0599999999999,0.));
#17827=CARTESIAN_POINT('',(93.4240705880017,39.5784009033024,0.));
#17828=CARTESIAN_POINT('',(94.9598704761907,38.3405617669895,0.));
#17829=CARTESIAN_POINT('',(92.0546631075751,38.2146694732975,0.));
#17830=CARTESIAN_POINT('Origin',(96.5599999999999,35.0599999999999,0.));
#17831=CARTESIAN_POINT('',(92.0546631075751,38.2146694732975,0.));
#17832=CARTESIAN_POINT('',(92.0546631075751,31.9053305267024,0.));
#17833=CARTESIAN_POINT('',(93.279438268468,33.4598704034959,0.));
#17834=CARTESIAN_POINT('',(93.4240705880018,30.5415990966974,0.));
#17835=CARTESIAN_POINT('Origin',(96.5599999999999,35.0599999999999,0.));
#17836=CARTESIAN_POINT('',(94.9598704761907,31.7794382330103,0.));
#17837=CARTESIAN_POINT('',(93.4240705880018,30.5415990966974,0.));
#17838=CARTESIAN_POINT('',(98.1601295238092,31.7794382330103,0.));
#17839=CARTESIAN_POINT('Origin',(96.5599999999999,35.0599999999999,0.));
#17840=CARTESIAN_POINT('',(99.6959294119981,30.5415990966974,0.));
#17841=CARTESIAN_POINT('',(98.1601295238092,31.7794382330103,0.));
#17842=CARTESIAN_POINT('',(101.065336892425,31.9053305267024,0.));
#17843=CARTESIAN_POINT('Origin',(96.5599999999999,35.0599999999999,0.));
#17844=CARTESIAN_POINT('',(99.8405617315319,33.459870403496,0.));
#17845=CARTESIAN_POINT('',(101.065336892425,31.9053305267024,0.));
#17846=CARTESIAN_POINT('',(99.8405617315319,36.6601295965039,0.));
#17847=CARTESIAN_POINT('Origin',(96.5599999999999,35.0599999999999,0.));
#17848=CARTESIAN_POINT('',(101.065336892425,38.2146694732975,0.));
#17849=CARTESIAN_POINT('',(99.8405617315319,36.6601295965039,0.));
#17850=CARTESIAN_POINT('',(99.6959294119981,39.5784009033024,0.));
#17851=CARTESIAN_POINT('Origin',(96.5599999999999,35.0599999999999,0.));
#17852=CARTESIAN_POINT('',(99.6959294119981,39.5784009033024,0.));
#17853=CARTESIAN_POINT('Origin',(95.6600000543452,29.0599999999999,380.));
#17854=CARTESIAN_POINT('',(96.5599999999999,29.5751481628425,380.));
#17855=CARTESIAN_POINT('',(95.6600000543452,29.0599999999999,380.));
#17856=CARTESIAN_POINT('Origin',(96.5599999999999,29.5751481628425,380.));
#17857=CARTESIAN_POINT('',(97.4599999456547,29.0599999999999,380.));
#17858=CARTESIAN_POINT('Origin',(97.4599999456547,29.0599999999999,380.));
#17859=CARTESIAN_POINT('',(100.764466193213,29.0599999999999,380.));
#17860=CARTESIAN_POINT('Origin',(100.764466193213,29.0599999999999,380.));
#17861=CARTESIAN_POINT('',(104.810000327124,25.0100007629401,380.));
#17862=CARTESIAN_POINT('Origin',(104.810000327124,25.0100007629401,380.));
#17863=CARTESIAN_POINT('',(104.810000327124,22.4600011663401,380.));
#17864=CARTESIAN_POINT('Origin',(104.609999923724,22.4600011663401,380.));
#17865=CARTESIAN_POINT('',(104.609999923724,22.2600007629398,380.));
#17866=CARTESIAN_POINT('Origin',(104.609999923724,22.2600007629398,380.));
#17867=CARTESIAN_POINT('',(101.210000196921,22.2600007629398,380.));
#17868=CARTESIAN_POINT('Origin',(101.210000196921,21.6600005660189,380.));
#17869=CARTESIAN_POINT('',(100.61,21.6600005660189,380.));
#17870=CARTESIAN_POINT('Origin',(100.61,21.6600005660189,380.));
#17871=CARTESIAN_POINT('',(100.61,20.7600003735979,380.));
#17872=CARTESIAN_POINT('Origin',(100.810000373598,20.7600003735979,380.));
#17873=CARTESIAN_POINT('',(100.810000373598,20.5599999999999,380.));
#17874=CARTESIAN_POINT('Origin',(100.810000373598,20.5599999999999,380.));
#17875=CARTESIAN_POINT('',(100.910000144262,20.5599999999999,380.));
#17876=CARTESIAN_POINT('Origin',(100.910000144262,20.3600005800758,380.));
#17877=CARTESIAN_POINT('',(101.109999564186,20.3600005800758,380.));
#17878=CARTESIAN_POINT('Origin',(101.109999564186,20.3600005800758,380.));
#17879=CARTESIAN_POINT('',(101.109999564186,20.2600003810484,380.));
#17880=CARTESIAN_POINT('Origin',(101.309999945234,20.2600003810484,380.));
#17881=CARTESIAN_POINT('',(101.309999945234,20.0599999999999,380.));
#17882=CARTESIAN_POINT('Origin',(101.309999945234,20.0599999999999,380.));
#17883=CARTESIAN_POINT('',(109.560000346242,20.0599999999999,380.));
#17884=CARTESIAN_POINT('Origin',(109.560000346242,22.0599996537577,380.));
#17885=CARTESIAN_POINT('',(111.56,22.0599996537577,380.));
#17886=CARTESIAN_POINT('Origin',(111.56,22.0599996537577,380.));
#17887=CARTESIAN_POINT('',(111.56,30.3100004787476,380.));
#17888=CARTESIAN_POINT('Origin',(111.359999715809,30.3100004787476,380.));
#17889=CARTESIAN_POINT('',(111.359999715809,30.5100007629388,380.));
#17890=CARTESIAN_POINT('Origin',(111.359999715809,30.5100007629388,380.));
#17891=CARTESIAN_POINT('',(111.260000611316,30.5100007629388,380.));
#17892=CARTESIAN_POINT('Origin',(111.260000611316,30.71000104713,380.));
#17893=CARTESIAN_POINT('',(111.060000327124,30.71000104713,380.));
#17894=CARTESIAN_POINT('Origin',(111.060000327124,30.71000104713,380.));
#17895=CARTESIAN_POINT('',(111.060000327124,30.8100004787487,380.));
#17896=CARTESIAN_POINT('Origin',(110.860000042933,30.8100004787487,380.));
#17897=CARTESIAN_POINT('',(110.860000042933,31.0100007629399,380.));
#17898=CARTESIAN_POINT('Origin',(110.860000042933,31.0100007629399,380.));
#17899=CARTESIAN_POINT('',(109.959999939919,31.0100007629399,380.));
#17900=CARTESIAN_POINT('Origin',(109.959999939919,30.4100003872052,380.));
#17901=CARTESIAN_POINT('',(109.359999564184,30.4100003872052,380.));
#17902=CARTESIAN_POINT('Origin',(109.359999564184,30.4100003872052,380.));
#17903=CARTESIAN_POINT('',(109.359999564184,27.0100002841911,380.));
#17904=CARTESIAN_POINT('Origin',(109.159999279993,27.0100002841911,380.));
#17905=CARTESIAN_POINT('',(109.159999279993,26.8099999999999,380.));
#17906=CARTESIAN_POINT('Origin',(109.159999279993,26.8099999999999,380.));
#17907=CARTESIAN_POINT('',(106.609999564184,26.8099999999999,380.));
#17908=CARTESIAN_POINT('Origin',(106.609999564184,26.8099999999999,380.));
#17909=CARTESIAN_POINT('',(102.564465430273,30.8555341339111,380.));
#17910=CARTESIAN_POINT('Origin',(102.564465430273,30.8555341339111,380.));
#17911=CARTESIAN_POINT('',(102.564465430273,34.1600003814696,380.));
#17912=CARTESIAN_POINT('Origin',(102.564465430273,34.1600003814696,380.));
#17913=CARTESIAN_POINT('',(102.044852164282,35.0599999999999,380.));
#17914=CARTESIAN_POINT('Origin',(102.044852164282,35.0599999999999,380.));
#17915=CARTESIAN_POINT('',(102.564465430273,35.9599996185302,380.));
#17916=CARTESIAN_POINT('Origin',(102.564465430273,35.9599996185302,380.));
#17917=CARTESIAN_POINT('',(102.564465430273,39.2644658660888,380.));
#17918=CARTESIAN_POINT('Origin',(102.564465430273,39.2644658660888,380.));
#17919=CARTESIAN_POINT('',(106.609999564184,43.3099999999999,380.));
#17920=CARTESIAN_POINT('Origin',(106.609999564184,43.3099999999999,380.));
#17921=CARTESIAN_POINT('',(109.159999279993,43.3099999999999,380.));
#17922=CARTESIAN_POINT('Origin',(109.159999279993,43.1099997158087,380.));
#17923=CARTESIAN_POINT('',(109.359999564184,43.1099997158087,380.));
#17924=CARTESIAN_POINT('Origin',(109.359999564184,43.1099997158087,380.));
#17925=CARTESIAN_POINT('',(109.359999564184,39.7099996127947,380.));
#17926=CARTESIAN_POINT('Origin',(109.959999939919,39.7099996127947,380.));
#17927=CARTESIAN_POINT('',(109.959999939919,39.1099992370599,380.));
#17928=CARTESIAN_POINT('Origin',(109.959999939919,39.1099992370599,380.));
#17929=CARTESIAN_POINT('',(110.860000042933,39.1099992370599,380.));
#17930=CARTESIAN_POINT('Origin',(110.860000042933,39.3099995212511,380.));
#17931=CARTESIAN_POINT('',(111.060000327124,39.3099995212511,380.));
#17932=CARTESIAN_POINT('Origin',(111.060000327124,39.3099995212511,380.));
#17933=CARTESIAN_POINT('',(111.060000327124,39.4099989528698,380.));
#17934=CARTESIAN_POINT('Origin',(111.260000611316,39.4099989528698,380.));
#17935=CARTESIAN_POINT('',(111.260000611316,39.609999237061,380.));
#17936=CARTESIAN_POINT('Origin',(111.260000611316,39.609999237061,380.));
#17937=CARTESIAN_POINT('',(111.359999715809,39.609999237061,380.));
#17938=CARTESIAN_POINT('Origin',(111.359999715809,39.8099995212523,380.));
#17939=CARTESIAN_POINT('',(111.56,39.8099995212523,380.));
#17940=CARTESIAN_POINT('Origin',(111.56,39.8099995212523,380.));
#17941=CARTESIAN_POINT('',(111.56,48.0600003462421,380.));
#17942=CARTESIAN_POINT('Origin',(109.560000346242,48.0600003462421,380.));
#17943=CARTESIAN_POINT('',(109.560000346242,50.0599999999999,380.));
#17944=CARTESIAN_POINT('Origin',(109.560000346242,50.0599999999999,380.));
#17945=CARTESIAN_POINT('',(101.309999945234,50.0599999999999,380.));
#17946=CARTESIAN_POINT('Origin',(101.309999945234,49.8599996189514,380.));
#17947=CARTESIAN_POINT('',(101.109999564186,49.8599996189514,380.));
#17948=CARTESIAN_POINT('Origin',(101.109999564186,49.8599996189514,380.));
#17949=CARTESIAN_POINT('',(101.109999564186,49.759999419924,380.));
#17950=CARTESIAN_POINT('Origin',(100.910000144262,49.759999419924,380.));
#17951=CARTESIAN_POINT('',(100.910000144262,49.5599999999999,380.));
#17952=CARTESIAN_POINT('Origin',(100.910000144262,49.5599999999999,380.));
#17953=CARTESIAN_POINT('',(100.810000373598,49.5599999999999,380.));
#17954=CARTESIAN_POINT('Origin',(100.810000373598,49.3599996264019,380.));
#17955=CARTESIAN_POINT('',(100.61,49.3599996264019,380.));
#17956=CARTESIAN_POINT('Origin',(100.61,49.3599996264019,380.));
#17957=CARTESIAN_POINT('',(100.61,48.4599994339809,380.));
#17958=CARTESIAN_POINT('Origin',(101.210000196921,48.4599994339809,380.));
#17959=CARTESIAN_POINT('',(101.210000196921,47.85999923706,380.));
#17960=CARTESIAN_POINT('Origin',(101.210000196921,47.85999923706,380.));
#17961=CARTESIAN_POINT('',(104.609999923724,47.85999923706,380.));
#17962=CARTESIAN_POINT('Origin',(104.609999923724,47.6599988336597,380.));
#17963=CARTESIAN_POINT('',(104.810000327124,47.6599988336597,380.));
#17964=CARTESIAN_POINT('Origin',(104.810000327124,47.6599988336597,380.));
#17965=CARTESIAN_POINT('',(104.810000327124,45.1099992370597,380.));
#17966=CARTESIAN_POINT('Origin',(104.810000327124,45.1099992370597,380.));
#17967=CARTESIAN_POINT('',(100.764466193213,41.0599999999999,380.));
#17968=CARTESIAN_POINT('Origin',(100.764466193213,41.0599999999999,380.));
#17969=CARTESIAN_POINT('',(97.4599999456547,41.0599999999999,380.));
#17970=CARTESIAN_POINT('Origin',(97.4599999456547,41.0599999999999,380.));
#17971=CARTESIAN_POINT('',(96.5599999999999,40.5448518371574,380.));
#17972=CARTESIAN_POINT('Origin',(96.5599999999999,40.5448518371574,380.));
#17973=CARTESIAN_POINT('',(95.6600000543452,41.0599999999999,380.));
#17974=CARTESIAN_POINT('Origin',(95.6600000543452,41.0599999999999,380.));
#17975=CARTESIAN_POINT('',(92.3555338067866,41.0599999999999,380.));
#17976=CARTESIAN_POINT('Origin',(92.3555338067866,41.0599999999999,380.));
#17977=CARTESIAN_POINT('',(88.3099996728755,45.1099992370597,380.));
#17978=CARTESIAN_POINT('Origin',(88.3099996728755,45.1099992370597,380.));
#17979=CARTESIAN_POINT('',(88.3099996728755,47.6599988336597,380.));
#17980=CARTESIAN_POINT('Origin',(88.5100000762757,47.6599988336597,380.));
#17981=CARTESIAN_POINT('',(88.5100000762757,47.85999923706,380.));
#17982=CARTESIAN_POINT('Origin',(88.5100000762757,47.85999923706,380.));
#17983=CARTESIAN_POINT('',(91.9099998030791,47.85999923706,380.));
#17984=CARTESIAN_POINT('Origin',(91.9099998030791,48.4599994339809,380.));
#17985=CARTESIAN_POINT('',(92.5099999999999,48.4599994339809,380.));
#17986=CARTESIAN_POINT('Origin',(92.5099999999999,48.4599994339809,380.));
#17987=CARTESIAN_POINT('',(92.5099999999999,49.3599996264019,380.));
#17988=CARTESIAN_POINT('Origin',(92.309999626402,49.3599996264019,380.));
#17989=CARTESIAN_POINT('',(92.309999626402,49.5599999999999,380.));
#17990=CARTESIAN_POINT('Origin',(92.309999626402,49.5599999999999,380.));
#17991=CARTESIAN_POINT('',(92.2099998557381,49.5599999999999,380.));
#17992=CARTESIAN_POINT('Origin',(92.2099998557381,49.759999419924,380.));
#17993=CARTESIAN_POINT('',(92.010000435814,49.759999419924,380.));
#17994=CARTESIAN_POINT('Origin',(92.010000435814,49.759999419924,380.));
#17995=CARTESIAN_POINT('',(92.010000435814,49.8599996189514,380.));
#17996=CARTESIAN_POINT('Origin',(91.8100000547655,49.8599996189514,380.));
#17997=CARTESIAN_POINT('',(91.8100000547655,50.0599999999999,380.));
#17998=CARTESIAN_POINT('Origin',(91.8100000547655,50.0599999999999,380.));
#17999=CARTESIAN_POINT('',(83.5599996537577,50.0599999999999,380.));
#18000=CARTESIAN_POINT('Origin',(83.5599996537577,48.0600003462421,380.));
#18001=CARTESIAN_POINT('',(81.5599999999999,48.0600003462421,380.));
#18002=CARTESIAN_POINT('Origin',(81.5599999999999,48.0600003462421,380.));
#18003=CARTESIAN_POINT('',(81.5599999999999,39.8099995212522,380.));
#18004=CARTESIAN_POINT('Origin',(81.7600002841911,39.8099995212522,380.));
#18005=CARTESIAN_POINT('',(81.7600002841911,39.609999237061,380.));
#18006=CARTESIAN_POINT('Origin',(81.7600002841911,39.609999237061,380.));
#18007=CARTESIAN_POINT('',(81.8599993886842,39.609999237061,380.));
#18008=CARTESIAN_POINT('Origin',(81.8599993886842,39.4099989528698,380.));
#18009=CARTESIAN_POINT('',(82.0599996728754,39.4099989528698,380.));
#18010=CARTESIAN_POINT('Origin',(82.0599996728754,39.4099989528698,380.));
#18011=CARTESIAN_POINT('',(82.0599996728754,39.3099995212511,380.));
#18012=CARTESIAN_POINT('Origin',(82.2599999570666,39.3099995212511,380.));
#18013=CARTESIAN_POINT('',(82.2599999570666,39.1099992370599,380.));
#18014=CARTESIAN_POINT('Origin',(82.2599999570666,39.1099992370599,380.));
#18015=CARTESIAN_POINT('',(83.1600000600806,39.1099992370599,380.));
#18016=CARTESIAN_POINT('Origin',(83.1600000600806,39.7099996127947,380.));
#18017=CARTESIAN_POINT('',(83.7600004358154,39.7099996127947,380.));
#18018=CARTESIAN_POINT('Origin',(83.7600004358154,39.7099996127947,380.));
#18019=CARTESIAN_POINT('',(83.7600004358154,43.1099997158087,380.));
#18020=CARTESIAN_POINT('Origin',(83.9600007200066,43.1099997158087,380.));
#18021=CARTESIAN_POINT('',(83.9600007200066,43.3099999999999,380.));
#18022=CARTESIAN_POINT('Origin',(83.9600007200066,43.3099999999999,380.));
#18023=CARTESIAN_POINT('',(86.510000435816,43.3099999999999,380.));
#18024=CARTESIAN_POINT('Origin',(86.510000435816,43.3099999999999,380.));
#18025=CARTESIAN_POINT('',(90.5555345697271,39.2644658660888,380.));
#18026=CARTESIAN_POINT('Origin',(90.5555345697271,39.2644658660888,380.));
#18027=CARTESIAN_POINT('',(90.5555345697271,35.9599996185302,380.));
#18028=CARTESIAN_POINT('Origin',(90.5555345697271,35.9599996185302,380.));
#18029=CARTESIAN_POINT('',(91.0751478357183,35.0599999999999,380.));
#18030=CARTESIAN_POINT('Origin',(91.0751478357183,35.0599999999999,380.));
#18031=CARTESIAN_POINT('',(90.5555345697271,34.1600003814696,380.));
#18032=CARTESIAN_POINT('Origin',(90.5555345697271,34.1600003814696,380.));
#18033=CARTESIAN_POINT('',(90.5555345697271,30.8555341339111,380.));
#18034=CARTESIAN_POINT('Origin',(90.5555345697271,30.8555341339111,380.));
#18035=CARTESIAN_POINT('',(86.510000435816,26.8099999999999,380.));
#18036=CARTESIAN_POINT('Origin',(86.510000435816,26.8099999999999,380.));
#18037=CARTESIAN_POINT('',(83.9600007200066,26.8099999999999,380.));
#18038=CARTESIAN_POINT('Origin',(83.9600007200066,27.0100002841911,380.));
#18039=CARTESIAN_POINT('',(83.7600004358154,27.0100002841911,380.));
#18040=CARTESIAN_POINT('Origin',(83.7600004358154,27.0100002841911,380.));
#18041=CARTESIAN_POINT('',(83.7600004358154,30.4100003872052,380.));
#18042=CARTESIAN_POINT('Origin',(83.1600000600806,30.4100003872052,380.));
#18043=CARTESIAN_POINT('',(83.1600000600806,31.0100007629399,380.));
#18044=CARTESIAN_POINT('Origin',(83.1600000600806,31.0100007629399,380.));
#18045=CARTESIAN_POINT('',(82.2599999570666,31.0100007629399,380.));
#18046=CARTESIAN_POINT('Origin',(82.2599999570666,30.8100004787487,380.));
#18047=CARTESIAN_POINT('',(82.0599996728754,30.8100004787487,380.));
#18048=CARTESIAN_POINT('Origin',(82.0599996728754,30.8100004787487,380.));
#18049=CARTESIAN_POINT('',(82.0599996728754,30.71000104713,380.));
#18050=CARTESIAN_POINT('Origin',(81.8599993886842,30.71000104713,380.));
#18051=CARTESIAN_POINT('',(81.8599993886842,30.5100007629388,380.));
#18052=CARTESIAN_POINT('Origin',(81.8599993886842,30.5100007629388,380.));
#18053=CARTESIAN_POINT('',(81.7600002841911,30.5100007629388,380.));
#18054=CARTESIAN_POINT('Origin',(81.7600002841911,30.3100004787476,380.));
#18055=CARTESIAN_POINT('',(81.5599999999999,30.3100004787476,380.));
#18056=CARTESIAN_POINT('Origin',(81.5599999999999,30.3100004787476,380.));
#18057=CARTESIAN_POINT('',(81.5599999999999,22.0599996537577,380.));
#18058=CARTESIAN_POINT('Origin',(83.5599996537577,22.0599996537577,380.));
#18059=CARTESIAN_POINT('',(83.5599996537578,20.0599999999999,380.));
#18060=CARTESIAN_POINT('Origin',(83.5599996537578,20.0599999999999,380.));
#18061=CARTESIAN_POINT('',(91.8100000547655,20.0599999999999,380.));
#18062=CARTESIAN_POINT('Origin',(91.8100000547655,20.2600003810484,380.));
#18063=CARTESIAN_POINT('',(92.010000435814,20.2600003810484,380.));
#18064=CARTESIAN_POINT('Origin',(92.010000435814,20.2600003810484,380.));
#18065=CARTESIAN_POINT('',(92.010000435814,20.3600005800758,380.));
#18066=CARTESIAN_POINT('Origin',(92.2099998557381,20.3600005800758,380.));
#18067=CARTESIAN_POINT('',(92.2099998557381,20.5599999999999,380.));
#18068=CARTESIAN_POINT('Origin',(92.2099998557381,20.5599999999999,380.));
#18069=CARTESIAN_POINT('',(92.309999626402,20.5599999999999,380.));
#18070=CARTESIAN_POINT('Origin',(92.309999626402,20.7600003735979,380.));
#18071=CARTESIAN_POINT('',(92.5099999999999,20.7600003735979,380.));
#18072=CARTESIAN_POINT('Origin',(92.5099999999999,20.7600003735979,380.));
#18073=CARTESIAN_POINT('',(92.5099999999999,21.6600005660189,380.));
#18074=CARTESIAN_POINT('Origin',(91.9099998030791,21.6600005660189,380.));
#18075=CARTESIAN_POINT('',(91.9099998030791,22.2600007629398,380.));
#18076=CARTESIAN_POINT('Origin',(91.9099998030791,22.2600007629398,380.));
#18077=CARTESIAN_POINT('',(88.5100000762757,22.2600007629398,380.));
#18078=CARTESIAN_POINT('Origin',(88.5100000762757,22.4600011663401,380.));
#18079=CARTESIAN_POINT('',(88.3099996728755,22.4600011663401,380.));
#18080=CARTESIAN_POINT('Origin',(88.3099996728755,22.4600011663401,380.));
#18081=CARTESIAN_POINT('',(88.3099996728755,25.0100007629401,380.));
#18082=CARTESIAN_POINT('Origin',(88.3099996728755,25.0100007629401,380.));
#18083=CARTESIAN_POINT('',(92.3555338067866,29.0599999999999,380.));
#18084=CARTESIAN_POINT('Origin',(92.3555338067866,29.0599999999999,380.));
#18085=CARTESIAN_POINT('Origin',(109.260001099622,47.7600004079674,380.));
#18086=CARTESIAN_POINT('',(110.260001090064,47.7600003984092,380.));
#18087=CARTESIAN_POINT('',(109.260001090064,48.7600003984092,380.));
#18088=CARTESIAN_POINT('Origin',(109.260001090064,48.7600003984092,380.));
#18089=CARTESIAN_POINT('',(107.060000327124,48.7600003984092,380.));
#18090=CARTESIAN_POINT('Origin',(107.060000317566,47.7600004079674,380.));
#18091=CARTESIAN_POINT('',(106.060000327124,47.7600003984092,380.));
#18092=CARTESIAN_POINT('Origin',(106.060000327124,47.7600003984092,380.));
#18093=CARTESIAN_POINT('',(106.060000327124,45.5599996354697,380.));
#18094=CARTESIAN_POINT('Origin',(107.060000317566,45.5599996259115,380.));
#18095=CARTESIAN_POINT('',(107.060000327124,44.5599996354697,380.));
#18096=CARTESIAN_POINT('Origin',(107.060000327124,44.5599996354697,380.));
#18097=CARTESIAN_POINT('',(109.260001090064,44.5599996354697,380.));
#18098=CARTESIAN_POINT('Origin',(109.260001099622,45.5599996259115,380.));
#18099=CARTESIAN_POINT('',(110.260001090064,45.5599996354697,380.));
#18100=CARTESIAN_POINT('Origin',(110.260001090064,45.5599996354697,380.));
#18101=CARTESIAN_POINT('Origin',(96.5599999999999,35.0599999999999,380.));
#18102=CARTESIAN_POINT('',(98.1601295238092,38.3405617669895,380.));
#18103=CARTESIAN_POINT('',(94.9598704761907,38.3405617669895,380.));
#18104=CARTESIAN_POINT('Origin',(94.9598704761907,38.3405617669895,380.));
#18105=CARTESIAN_POINT('',(93.4240705880017,39.5784009033024,380.));
#18106=CARTESIAN_POINT('Origin',(96.5599999999999,35.0599999999999,380.));
#18107=CARTESIAN_POINT('',(92.0546631075751,38.2146694732975,380.));
#18108=CARTESIAN_POINT('Origin',(92.0546631075751,38.2146694732975,380.));
#18109=CARTESIAN_POINT('Origin',(93.279438268468,33.4598704034959,380.));
#18110=CARTESIAN_POINT('',(92.0546631075751,31.9053305267024,380.));
#18111=CARTESIAN_POINT('Origin',(96.5599999999999,35.0599999999999,380.));
#18112=CARTESIAN_POINT('',(93.4240705880018,30.5415990966974,380.));
#18113=CARTESIAN_POINT('Origin',(93.4240705880018,30.5415990966974,380.));
#18114=CARTESIAN_POINT('',(94.9598704761907,31.7794382330103,380.));
#18115=CARTESIAN_POINT('Origin',(96.5599999999999,35.0599999999999,380.));
#18116=CARTESIAN_POINT('',(98.1601295238092,31.7794382330103,380.));
#18117=CARTESIAN_POINT('Origin',(98.1601295238092,31.7794382330103,380.));
#18118=CARTESIAN_POINT('',(99.6959294119981,30.5415990966974,380.));
#18119=CARTESIAN_POINT('Origin',(96.5599999999999,35.0599999999999,380.));
#18120=CARTESIAN_POINT('',(101.065336892425,31.9053305267024,380.));
#18121=CARTESIAN_POINT('Origin',(101.065336892425,31.9053305267024,380.));
#18122=CARTESIAN_POINT('',(99.8405617315319,33.459870403496,380.));
#18123=CARTESIAN_POINT('Origin',(96.5599999999999,35.0599999999999,380.));
#18124=CARTESIAN_POINT('',(99.8405617315319,36.6601295965039,380.));
#18125=CARTESIAN_POINT('Origin',(99.8405617315319,36.6601295965039,380.));
#18126=CARTESIAN_POINT('',(101.065336892425,38.2146694732975,380.));
#18127=CARTESIAN_POINT('Origin',(96.5599999999999,35.0599999999999,380.));
#18128=CARTESIAN_POINT('',(99.6959294119981,39.5784009033024,380.));
#18129=CARTESIAN_POINT('Origin',(99.6959294119981,39.5784009033024,380.));
#18130=CARTESIAN_POINT('Origin',(83.8599989003778,22.3599995920324,380.));
#18131=CARTESIAN_POINT('',(82.8599989099361,22.3599996015906,380.));
#18132=CARTESIAN_POINT('',(83.859998909936,21.3599996015906,380.));
#18133=CARTESIAN_POINT('Origin',(83.859998909936,21.3599996015906,380.));
#18134=CARTESIAN_POINT('',(86.0599996728755,21.3599996015906,380.));
#18135=CARTESIAN_POINT('Origin',(86.0599996824337,22.3599995920324,380.));
#18136=CARTESIAN_POINT('',(87.0599996728755,22.3599996015906,380.));
#18137=CARTESIAN_POINT('Origin',(87.0599996728755,22.3599996015906,380.));
#18138=CARTESIAN_POINT('',(87.0599996728755,24.5600003645301,380.));
#18139=CARTESIAN_POINT('Origin',(86.0599996824337,24.5600003740883,380.));
#18140=CARTESIAN_POINT('',(86.0599996728755,25.5600003645301,380.));
#18141=CARTESIAN_POINT('Origin',(86.0599996728755,25.5600003645301,380.));
#18142=CARTESIAN_POINT('',(83.859998909936,25.5600003645301,380.));
#18143=CARTESIAN_POINT('Origin',(83.8599989003778,24.5600003740883,380.));
#18144=CARTESIAN_POINT('',(82.8599989099361,24.5600003645301,380.));
#18145=CARTESIAN_POINT('Origin',(82.859998909936,24.5600003645301,380.));
#18146=CARTESIAN_POINT('Origin',(109.260001099622,22.3599995920324,380.));
#18147=CARTESIAN_POINT('',(109.260001090064,21.3599996015906,380.));
#18148=CARTESIAN_POINT('',(110.260001090064,22.3599996015906,380.));
#18149=CARTESIAN_POINT('Origin',(110.260001090064,22.3599996015906,380.));
#18150=CARTESIAN_POINT('',(110.260001090064,24.5600003645301,380.));
#18151=CARTESIAN_POINT('Origin',(109.260001099622,24.5600003740883,380.));
#18152=CARTESIAN_POINT('',(109.260001090064,25.5600003645301,380.));
#18153=CARTESIAN_POINT('Origin',(109.260001090064,25.5600003645301,380.));
#18154=CARTESIAN_POINT('',(107.060000327124,25.5600003645301,380.));
#18155=CARTESIAN_POINT('Origin',(107.060000317566,24.5600003740883,380.));
#18156=CARTESIAN_POINT('',(106.060000327124,24.5600003645301,380.));
#18157=CARTESIAN_POINT('Origin',(106.060000327124,24.5600003645301,380.));
#18158=CARTESIAN_POINT('',(106.060000327124,22.3599996015906,380.));
#18159=CARTESIAN_POINT('Origin',(107.060000317566,22.3599995920324,380.));
#18160=CARTESIAN_POINT('',(107.060000327124,21.3599996015906,380.));
#18161=CARTESIAN_POINT('Origin',(107.060000327124,21.3599996015906,380.));
#18162=CARTESIAN_POINT('Origin',(86.0599996824337,47.7600004079674,380.));
#18163=CARTESIAN_POINT('',(87.0599996728755,47.7600003984092,380.));
#18164=CARTESIAN_POINT('',(86.0599996728755,48.7600003984092,380.));
#18165=CARTESIAN_POINT('Origin',(86.0599996728755,48.7600003984092,380.));
#18166=CARTESIAN_POINT('',(83.859998909936,48.7600003984092,380.));
#18167=CARTESIAN_POINT('Origin',(83.8599989003778,47.7600004079674,380.));
#18168=CARTESIAN_POINT('',(82.8599989099361,47.7600003984092,380.));
#18169=CARTESIAN_POINT('Origin',(82.859998909936,47.7600003984092,380.));
#18170=CARTESIAN_POINT('',(82.8599989099361,45.5599996354697,380.));
#18171=CARTESIAN_POINT('Origin',(83.8599989003778,45.5599996259115,380.));
#18172=CARTESIAN_POINT('',(83.8599989099361,44.5599996354697,380.));
#18173=CARTESIAN_POINT('Origin',(83.8599989099361,44.5599996354697,380.));
#18174=CARTESIAN_POINT('',(86.0599996728755,44.5599996354697,380.));
#18175=CARTESIAN_POINT('Origin',(86.0599996824337,45.5599996259115,380.));
#18176=CARTESIAN_POINT('',(87.0599996728755,45.5599996354697,380.));
#18177=CARTESIAN_POINT('Origin',(87.0599996728755,45.5599996354697,380.));
#18178=CARTESIAN_POINT('',(0.,0.,0.));
#18179=CARTESIAN_POINT('Origin',(10.,0.,16.));
#18180=CARTESIAN_POINT('',(-6.,-2.75545529808154E-16,13.75));
#18181=CARTESIAN_POINT('Origin',(-6.00000000000001,0.,16.));
#18182=CARTESIAN_POINT('',(-12.,-2.75545529808154E-16,13.75));
#18183=CARTESIAN_POINT('',(10.,-2.75545529808154E-16,13.75));
#18184=CARTESIAN_POINT('Origin',(-12.,0.,16.));
#18185=CARTESIAN_POINT('Origin',(10.,-3.91886975727153E-15,-16.));
#18186=CARTESIAN_POINT('',(12.,-4.19441528707969E-15,-18.25));
#18187=CARTESIAN_POINT('Origin',(12.,-3.91886975727153E-15,-16.));
#18188=CARTESIAN_POINT('',(6.,-4.19441528707969E-15,-18.25));
#18189=CARTESIAN_POINT('',(10.,-4.19441528707969E-15,-18.25));
#18190=CARTESIAN_POINT('Origin',(6.,-3.91886975727153E-15,-16.));
#18191=CARTESIAN_POINT('Origin',(10.,13.,0.));
#18192=CARTESIAN_POINT('',(10.,13.,8.));
#18193=CARTESIAN_POINT('',(10.,13.,-17.));
#18194=CARTESIAN_POINT('',(10.,13.,0.));
#18195=CARTESIAN_POINT('',(10.,3.95,8.));
#18196=CARTESIAN_POINT('',(10.,3.95,8.));
#18197=CARTESIAN_POINT('',(10.,3.95,-22.));
#18198=CARTESIAN_POINT('',(10.,3.95,0.));
#18199=CARTESIAN_POINT('',(10.,8.,-22.));
#18200=CARTESIAN_POINT('',(10.,13.,-22.));
#18201=CARTESIAN_POINT('Origin',(10.,8.,-17.));
#18202=CARTESIAN_POINT('Origin',(-10.,13.,0.));
#18203=CARTESIAN_POINT('',(-10.,13.,17.));
#18204=CARTESIAN_POINT('',(-10.,13.,-8.));
#18205=CARTESIAN_POINT('',(-10.,13.,0.));
#18206=CARTESIAN_POINT('',(-10.,3.95,-8.));
#18207=CARTESIAN_POINT('',(-10.,3.95,-8.));
#18208=CARTESIAN_POINT('',(-10.,3.95,22.));
#18209=CARTESIAN_POINT('',(-10.,3.95,0.));
#18210=CARTESIAN_POINT('',(-10.,8.,22.));
#18211=CARTESIAN_POINT('',(-10.,13.,22.));
#18212=CARTESIAN_POINT('Origin',(-10.,8.,17.));
#18213=CARTESIAN_POINT('Origin',(-10.,13.,0.));
#18214=CARTESIAN_POINT('',(-10.,-3.95,-8.));
#18215=CARTESIAN_POINT('',(-10.,-3.95,22.));
#18216=CARTESIAN_POINT('',(-10.,-3.95,0.));
#18217=CARTESIAN_POINT('',(-10.,-13.,-8.));
#18218=CARTESIAN_POINT('',(-10.,-13.,-8.));
#18219=CARTESIAN_POINT('',(-10.,-13.,17.));
#18220=CARTESIAN_POINT('',(-10.,-13.,0.));
#18221=CARTESIAN_POINT('',(-10.,-7.99999999999999,22.));
#18222=CARTESIAN_POINT('Origin',(-10.,-8.,17.));
#18223=CARTESIAN_POINT('',(-10.,13.,22.));
#18224=CARTESIAN_POINT('Origin',(0.,13.,22.));
#18225=CARTESIAN_POINT('',(-12.,3.95,22.));
#18226=CARTESIAN_POINT('',(-12.,3.95,22.));
#18227=CARTESIAN_POINT('',(-12.,-3.95,22.));
#18228=CARTESIAN_POINT('',(-12.,0.,22.));
#18229=CARTESIAN_POINT('',(-12.,-3.95,22.));
#18230=CARTESIAN_POINT('',(-6.00000000000001,-7.99999999999999,22.));
#18231=CARTESIAN_POINT('',(0.,-8.,22.));
#18232=CARTESIAN_POINT('',(-6.00000000000001,8.,22.));
#18233=CARTESIAN_POINT('',(-6.00000000000001,13.,22.));
#18234=CARTESIAN_POINT('',(-10.,8.,22.));
#18235=CARTESIAN_POINT('Origin',(-6.,13.,-2.60208521396521E-15));
#18236=CARTESIAN_POINT('',(-6.00000000000001,-13.,17.));
#18237=CARTESIAN_POINT('Origin',(-6.00000000000001,-8.,17.));
#18238=CARTESIAN_POINT('',(-6.,-13.,12.));
#18239=CARTESIAN_POINT('',(-6.,-13.,-2.60208521396521E-15));
#18240=CARTESIAN_POINT('',(-6.,13.,12.));
#18241=CARTESIAN_POINT('',(-6.,13.,12.));
#18242=CARTESIAN_POINT('',(-6.00000000000001,13.,17.));
#18243=CARTESIAN_POINT('',(-6.,13.,-2.60208521396521E-15));
#18244=CARTESIAN_POINT('Origin',(-6.00000000000001,8.,17.));
#18245=CARTESIAN_POINT('Origin',(1.73472347597681E-15,13.,10.));
#18246=CARTESIAN_POINT('',(8.,-13.,10.));
#18247=CARTESIAN_POINT('',(-4.,-13.,10.));
#18248=CARTESIAN_POINT('',(1.73472347597681E-15,-13.,10.));
#18249=CARTESIAN_POINT('',(8.,-3.95,10.));
#18250=CARTESIAN_POINT('',(8.,-3.95,10.));
#18251=CARTESIAN_POINT('',(10.,-3.95,10.));
#18252=CARTESIAN_POINT('',(12.,-3.95,10.));
#18253=CARTESIAN_POINT('',(10.,3.95,10.));
#18254=CARTESIAN_POINT('',(10.,13.,10.));
#18255=CARTESIAN_POINT('',(8.,3.95,10.));
#18256=CARTESIAN_POINT('',(12.,3.95,10.));
#18257=CARTESIAN_POINT('',(8.,13.,10.));
#18258=CARTESIAN_POINT('',(8.,13.,10.));
#18259=CARTESIAN_POINT('',(-4.,13.,10.));
#18260=CARTESIAN_POINT('',(1.73472347597681E-15,13.,10.));
#18261=CARTESIAN_POINT('',(-4.,-13.,10.));
#18262=CARTESIAN_POINT('Origin',(10.,13.,0.));
#18263=CARTESIAN_POINT('',(10.,-3.94999999999999,-22.));
#18264=CARTESIAN_POINT('',(10.,-3.95,8.));
#18265=CARTESIAN_POINT('',(10.,-3.95,0.));
#18266=CARTESIAN_POINT('',(10.,-13.,8.));
#18267=CARTESIAN_POINT('',(10.,-13.,8.));
#18268=CARTESIAN_POINT('',(10.,-13.,-17.));
#18269=CARTESIAN_POINT('',(10.,-13.,0.));
#18270=CARTESIAN_POINT('',(10.,-7.99999999999999,-22.));
#18271=CARTESIAN_POINT('Origin',(10.,-8.,-17.));
#18272=CARTESIAN_POINT('',(10.,13.,-22.));
#18273=CARTESIAN_POINT('Origin',(0.,13.,-22.));
#18274=CARTESIAN_POINT('',(6.,8.,-22.));
#18275=CARTESIAN_POINT('',(6.,-7.99999999999999,-22.));
#18276=CARTESIAN_POINT('',(6.,13.,-22.));
#18277=CARTESIAN_POINT('',(10.,8.,-22.));
#18278=CARTESIAN_POINT('',(12.,3.95,-22.));
#18279=CARTESIAN_POINT('',(12.,3.95,-22.));
#18280=CARTESIAN_POINT('',(12.,-3.95,-22.));
#18281=CARTESIAN_POINT('',(12.,0.,-22.));
#18282=CARTESIAN_POINT('',(12.,-3.95,-22.));
#18283=CARTESIAN_POINT('',(0.,-8.,-22.));
#18284=CARTESIAN_POINT('Origin',(6.,13.,0.));
#18285=CARTESIAN_POINT('',(6.,13.,-12.));
#18286=CARTESIAN_POINT('',(6.,13.,-17.));
#18287=CARTESIAN_POINT('',(6.,13.,0.));
#18288=CARTESIAN_POINT('Origin',(6.,8.,-17.));
#18289=CARTESIAN_POINT('',(6.,-13.,-17.));
#18290=CARTESIAN_POINT('Origin',(6.,-8.,-17.));
#18291=CARTESIAN_POINT('',(6.,-13.,-12.));
#18292=CARTESIAN_POINT('',(6.,-13.,0.));
#18293=CARTESIAN_POINT('',(6.,13.,-12.));
#18294=CARTESIAN_POINT('Origin',(0.,13.,-10.));
#18295=CARTESIAN_POINT('',(4.,-13.,-10.));
#18296=CARTESIAN_POINT('',(-8.,-13.,-10.));
#18297=CARTESIAN_POINT('',(0.,-13.,-10.));
#18298=CARTESIAN_POINT('',(-8.,-3.95,-10.));
#18299=CARTESIAN_POINT('',(-8.,-3.95,-10.));
#18300=CARTESIAN_POINT('',(-10.,-3.95,-10.));
#18301=CARTESIAN_POINT('',(-12.,-3.95,-10.));
#18302=CARTESIAN_POINT('',(-10.,3.95,-10.));
#18303=CARTESIAN_POINT('',(-10.,3.95,-10.));
#18304=CARTESIAN_POINT('',(-8.,3.95,-10.));
#18305=CARTESIAN_POINT('',(-12.,3.95,-10.));
#18306=CARTESIAN_POINT('',(-8.,13.,-10.));
#18307=CARTESIAN_POINT('',(-8.,13.,-10.));
#18308=CARTESIAN_POINT('',(4.,13.,-10.));
#18309=CARTESIAN_POINT('',(0.,13.,-10.));
#18310=CARTESIAN_POINT('',(4.,13.,-10.));
#18311=CARTESIAN_POINT('Origin',(0.,13.,0.));
#18312=CARTESIAN_POINT('Origin',(-8.,13.,-8.));
#18313=CARTESIAN_POINT('',(-6.00000000000001,13.,17.));
#18314=CARTESIAN_POINT('Origin',(-4.,13.,12.));
#18315=CARTESIAN_POINT('Origin',(8.,13.,8.));
#18316=CARTESIAN_POINT('',(6.,13.,-17.));
#18317=CARTESIAN_POINT('Origin',(4.,13.,-12.));
#18318=CARTESIAN_POINT('',(-4.,13.,-4.));
#18319=CARTESIAN_POINT('',(-4.,13.,4.));
#18320=CARTESIAN_POINT('Origin',(-4.,13.,0.));
#18321=CARTESIAN_POINT('',(4.,13.,-4.));
#18322=CARTESIAN_POINT('',(-4.,13.,-4.));
#18323=CARTESIAN_POINT('',(4.,13.,4.));
#18324=CARTESIAN_POINT('Origin',(4.,13.,-1.46957615897682E-15));
#18325=CARTESIAN_POINT('',(-4.,13.,4.));
#18326=CARTESIAN_POINT('Origin',(0.,-13.,0.));
#18327=CARTESIAN_POINT('Origin',(-8.,-13.,-8.));
#18328=CARTESIAN_POINT('Origin',(4.,-13.,-12.));
#18329=CARTESIAN_POINT('',(0.,-13.,-17.));
#18330=CARTESIAN_POINT('Origin',(8.,-13.,8.));
#18331=CARTESIAN_POINT('Origin',(-4.,-13.,12.));
#18332=CARTESIAN_POINT('',(0.,-13.,17.));
#18333=CARTESIAN_POINT('',(4.,-13.,-4.));
#18334=CARTESIAN_POINT('',(-4.,-13.,-4.));
#18335=CARTESIAN_POINT('',(-4.,-13.,-4.));
#18336=CARTESIAN_POINT('',(-4.,-13.,4.));
#18337=CARTESIAN_POINT('Origin',(-4.,-13.,0.));
#18338=CARTESIAN_POINT('',(4.,-13.,4.));
#18339=CARTESIAN_POINT('',(-4.,-13.,4.));
#18340=CARTESIAN_POINT('Origin',(4.,-13.,-1.46957615897682E-15));
#18341=CARTESIAN_POINT('Origin',(-4.,-13.,0.));
#18342=CARTESIAN_POINT('',(-4.,-13.,4.));
#18343=CARTESIAN_POINT('',(-4.,-13.,-4.));
#18344=CARTESIAN_POINT('Origin',(-4.,-13.,-4.));
#18345=CARTESIAN_POINT('',(4.,-13.,-4.));
#18346=CARTESIAN_POINT('Origin',(4.,-13.,-1.46957615897682E-15));
#18347=CARTESIAN_POINT('',(4.,-13.,4.));
#18348=CARTESIAN_POINT('Origin',(-4.,-13.,4.));
#18349=CARTESIAN_POINT('Origin',(4.,13.,-12.));
#18350=CARTESIAN_POINT('Origin',(-4.,13.,12.));
#18351=CARTESIAN_POINT('Origin',(0.,8.,-17.));
#18352=CARTESIAN_POINT('Origin',(0.,-8.,-17.));
#18353=CARTESIAN_POINT('Origin',(0.,-8.,17.));
#18354=CARTESIAN_POINT('Origin',(0.,8.,17.));
#18355=CARTESIAN_POINT('Origin',(-12.,3.95,0.));
#18356=CARTESIAN_POINT('Origin',(-8.,3.95,-8.));
#18357=CARTESIAN_POINT('',(-12.,3.95,-8.));
#18358=CARTESIAN_POINT('Origin',(-10.,3.95,-8.));
#18359=CARTESIAN_POINT('',(-12.,3.95,0.));
#18360=CARTESIAN_POINT('Origin',(-12.,-3.95,0.));
#18361=CARTESIAN_POINT('',(-12.,-3.95,-8.));
#18362=CARTESIAN_POINT('',(-12.,-3.95,0.));
#18363=CARTESIAN_POINT('Origin',(-10.,-3.95,-8.));
#18364=CARTESIAN_POINT('Origin',(-8.,-3.95,-8.));
#18365=CARTESIAN_POINT('Origin',(-12.,0.,0.));
#18366=CARTESIAN_POINT('',(-12.,-3.95,-8.));
#18367=CARTESIAN_POINT('Origin',(12.,3.95,0.));
#18368=CARTESIAN_POINT('Origin',(8.,3.95,8.));
#18369=CARTESIAN_POINT('',(12.,3.95,8.));
#18370=CARTESIAN_POINT('Origin',(10.,3.95,8.));
#18371=CARTESIAN_POINT('',(12.,3.95,0.));
#18372=CARTESIAN_POINT('Origin',(12.,-3.95,0.));
#18373=CARTESIAN_POINT('',(12.,-3.95,8.));
#18374=CARTESIAN_POINT('',(12.,-3.95,0.));
#18375=CARTESIAN_POINT('Origin',(10.,-3.95,8.));
#18376=CARTESIAN_POINT('Origin',(8.,-3.95,8.));
#18377=CARTESIAN_POINT('Origin',(12.,0.,0.));
#18378=CARTESIAN_POINT('',(12.,0.,8.));
#18379=CARTESIAN_POINT('Origin',(-8.,13.,-8.));
#18380=CARTESIAN_POINT('Origin',(-10.,13.,-8.));
#18381=CARTESIAN_POINT('Origin',(-8.,13.,-8.));
#18382=CARTESIAN_POINT('Origin',(8.,13.,8.));
#18383=CARTESIAN_POINT('Origin',(10.,13.,8.));
#18384=CARTESIAN_POINT('Origin',(8.,13.,8.));
#18385=CARTESIAN_POINT('',(0.,0.,0.));
#18386=CARTESIAN_POINT('Origin',(0.,17.,6.));
#18387=CARTESIAN_POINT('',(-3.99999999999999,17.,1.6));
#18388=CARTESIAN_POINT('Origin',(0.,17.,1.6));
#18389=CARTESIAN_POINT('',(-3.99999999999999,17.,6.));
#18390=CARTESIAN_POINT('',(-3.99999999999999,17.,6.));
#18391=CARTESIAN_POINT('Origin',(0.,17.,6.));
#18392=CARTESIAN_POINT('Origin',(0.,17.,6.));
#18393=CARTESIAN_POINT('',(-2.15,17.,-2.));
#18394=CARTESIAN_POINT('Origin',(0.,17.,-2.));
#18395=CARTESIAN_POINT('',(-2.15,17.,1.6));
#18396=CARTESIAN_POINT('',(-2.15,17.,6.));
#18397=CARTESIAN_POINT('Origin',(0.,17.,1.6));
#18398=CARTESIAN_POINT('Origin',(0.,0.,0.));
#18399=CARTESIAN_POINT('',(-10.,26.,0.));
#18400=CARTESIAN_POINT('',(-10.,20.95,0.));
#18401=CARTESIAN_POINT('',(-10.,-30.,0.));
#18402=CARTESIAN_POINT('',(-6.,30.,0.));
#18403=CARTESIAN_POINT('Origin',(-6.,26.,0.));
#18404=CARTESIAN_POINT('',(6.,30.,0.));
#18405=CARTESIAN_POINT('',(10.,30.,0.));
#18406=CARTESIAN_POINT('',(10.,26.,0.));
#18407=CARTESIAN_POINT('Origin',(6.,26.,0.));
#18408=CARTESIAN_POINT('',(10.,20.95,0.));
#18409=CARTESIAN_POINT('',(10.,-30.,0.));
#18410=CARTESIAN_POINT('',(10.,20.95,0.));
#18411=CARTESIAN_POINT('Origin',(0.,0.,0.));
#18412=CARTESIAN_POINT('',(10.,13.05,0.));
#18413=CARTESIAN_POINT('',(-10.,13.05,0.));
#18414=CARTESIAN_POINT('',(10.,13.05,0.));
#18415=CARTESIAN_POINT('',(10.,-30.,0.));
#18416=CARTESIAN_POINT('',(10.,-30.,0.));
#18417=CARTESIAN_POINT('',(4.00000000000001,-30.,0.));
#18418=CARTESIAN_POINT('',(10.,-30.,0.));
#18419=CARTESIAN_POINT('',(4.00000000000001,-36.,4.54060943916541E-16));
#18420=CARTESIAN_POINT('',(4.00000000000001,-36.,4.54060943916541E-16));
#18421=CARTESIAN_POINT('',(-3.99999999999999,-36.,4.54060943815567E-16));
#18422=CARTESIAN_POINT('',(4.00000000000001,-36.,4.54060943916541E-16));
#18423=CARTESIAN_POINT('',(-3.99999999999999,-30.,0.));
#18424=CARTESIAN_POINT('',(-3.99999999999999,-36.,4.54060943815567E-16));
#18425=CARTESIAN_POINT('',(-10.,-30.,0.));
#18426=CARTESIAN_POINT('',(10.,-30.,0.));
#18427=CARTESIAN_POINT('',(-10.,-30.,0.));
#18428=CARTESIAN_POINT('Origin',(10.,-30.,6.));
#18429=CARTESIAN_POINT('',(-3.99999999999999,-30.,6.));
#18430=CARTESIAN_POINT('',(-3.99999999999999,-30.,4.54060943815567E-16));
#18431=CARTESIAN_POINT('',(-10.,-30.,6.));
#18432=CARTESIAN_POINT('',(10.,-30.,6.));
#18433=CARTESIAN_POINT('',(-10.,-30.,6.));
#18434=CARTESIAN_POINT('Origin',(10.,-30.,6.));
#18435=CARTESIAN_POINT('',(4.00000000000001,-30.,6.));
#18436=CARTESIAN_POINT('',(4.00000000000001,-30.,4.54060943916541E-16));
#18437=CARTESIAN_POINT('',(10.,-30.,6.));
#18438=CARTESIAN_POINT('',(10.,-30.,6.));
#18439=CARTESIAN_POINT('',(10.,-30.,6.));
#18440=CARTESIAN_POINT('Origin',(-10.,-30.,6.));
#18441=CARTESIAN_POINT('',(-10.,26.,6.));
#18442=CARTESIAN_POINT('',(-10.,-30.,6.));
#18443=CARTESIAN_POINT('',(-10.,26.,6.));
#18444=CARTESIAN_POINT('',(-10.,20.95,-2.));
#18445=CARTESIAN_POINT('',(-10.,20.95,-2.));
#18446=CARTESIAN_POINT('',(-10.,13.05,-2.));
#18447=CARTESIAN_POINT('',(-10.,20.95,-2.));
#18448=CARTESIAN_POINT('',(-10.,13.05,-2.));
#18449=CARTESIAN_POINT('Origin',(10.,-30.,6.));
#18450=CARTESIAN_POINT('',(10.,26.,6.));
#18451=CARTESIAN_POINT('',(10.,26.,6.));
#18452=CARTESIAN_POINT('',(10.,-30.,6.));
#18453=CARTESIAN_POINT('',(10.,13.05,-2.));
#18454=CARTESIAN_POINT('',(10.,13.05,-2.));
#18455=CARTESIAN_POINT('',(10.,20.95,-2.));
#18456=CARTESIAN_POINT('',(10.,20.95,-2.));
#18457=CARTESIAN_POINT('',(10.,20.95,-2.));
#18458=CARTESIAN_POINT('Origin',(10.,30.,6.));
#18459=CARTESIAN_POINT('',(-6.,30.,6.));
#18460=CARTESIAN_POINT('',(-6.,30.,6.));
#18461=CARTESIAN_POINT('',(6.,30.,6.));
#18462=CARTESIAN_POINT('',(10.,30.,6.));
#18463=CARTESIAN_POINT('',(6.,30.,6.));
#18464=CARTESIAN_POINT('Origin',(0.,0.,6.));
#18465=CARTESIAN_POINT('Origin',(-6.,26.,6.));
#18466=CARTESIAN_POINT('',(-3.99999999999999,-36.,6.));
#18467=CARTESIAN_POINT('',(-3.99999999999999,-36.,6.));
#18468=CARTESIAN_POINT('',(4.00000000000001,-36.,6.));
#18469=CARTESIAN_POINT('',(4.00000000000001,-36.,6.));
#18470=CARTESIAN_POINT('',(4.00000000000001,-36.,6.));
#18471=CARTESIAN_POINT('Origin',(6.,26.,6.));
#18472=CARTESIAN_POINT('Origin',(-3.99999999999999,-36.,4.54060943815567E-16));
#18473=CARTESIAN_POINT('',(-3.99999999999999,-36.,4.54060943815567E-16));
#18474=CARTESIAN_POINT('Origin',(4.00000000000001,-36.,4.54060943916541E-16));
#18475=CARTESIAN_POINT('',(4.00000000000001,-36.,4.54060943916541E-16));
#18476=CARTESIAN_POINT('Origin',(5.20417042793042E-16,-36.,0.));
#18477=CARTESIAN_POINT('Origin',(10.,13.05,-2.));
#18478=CARTESIAN_POINT('',(10.,13.05,-2.));
#18479=CARTESIAN_POINT('Origin',(10.,20.95,-2.));
#18480=CARTESIAN_POINT('',(10.,20.95,-2.));
#18481=CARTESIAN_POINT('Origin',(0.,0.,-2.));
#18482=CARTESIAN_POINT('Origin',(-6.,26.,6.));
#18483=CARTESIAN_POINT('Origin',(6.,26.,6.));
#18484=CARTESIAN_POINT('Origin',(2.15,17.,1.6));
#18485=CARTESIAN_POINT('',(0.,0.,0.));
#18486=CARTESIAN_POINT('Origin',(0.,6.,0.));
#18487=CARTESIAN_POINT('',(11.,6.,-12.5));
#18488=CARTESIAN_POINT('',(-11.,6.,-12.5));
#18489=CARTESIAN_POINT('',(15.,6.,-12.5));
#18490=CARTESIAN_POINT('',(-15.,6.,-8.49999999999999));
#18491=CARTESIAN_POINT('Origin',(-11.,6.,-8.49999999999999));
#18492=CARTESIAN_POINT('',(-15.,6.,8.50000000000001));
#18493=CARTESIAN_POINT('',(-15.,6.,12.5));
#18494=CARTESIAN_POINT('',(-11.,6.,12.5));
#18495=CARTESIAN_POINT('Origin',(-11.,6.,8.50000000000001));
#18496=CARTESIAN_POINT('',(11.,6.,12.5));
#18497=CARTESIAN_POINT('',(15.,6.,12.5));
#18498=CARTESIAN_POINT('',(15.,6.,8.5));
#18499=CARTESIAN_POINT('Origin',(11.,6.,8.5));
#18500=CARTESIAN_POINT('',(15.,6.,-8.5));
#18501=CARTESIAN_POINT('',(15.,6.,12.5));
#18502=CARTESIAN_POINT('Origin',(11.,6.,-8.5));
#18503=CARTESIAN_POINT('',(-4.2,6.,3.2));
#18504=CARTESIAN_POINT('',(4.2,6.,3.2));
#18505=CARTESIAN_POINT('',(4.2,6.,3.2));
#18506=CARTESIAN_POINT('',(-4.2,6.,-3.2));
#18507=CARTESIAN_POINT('',(-4.2,6.,3.2));
#18508=CARTESIAN_POINT('',(4.2,6.,-3.2));
#18509=CARTESIAN_POINT('',(4.2,6.,-3.2));
#18510=CARTESIAN_POINT('',(4.2,6.,3.2));
#18511=CARTESIAN_POINT('Origin',(0.,0.,0.));
#18512=CARTESIAN_POINT('',(-15.,0.,-8.49999999999999));
#18513=CARTESIAN_POINT('',(-15.,0.,8.50000000000001));
#18514=CARTESIAN_POINT('',(-15.,0.,12.5));
#18515=CARTESIAN_POINT('',(-11.,0.,-12.5));
#18516=CARTESIAN_POINT('Origin',(-11.,0.,-8.49999999999999));
#18517=CARTESIAN_POINT('',(11.,0.,-12.5));
#18518=CARTESIAN_POINT('',(15.,0.,-12.5));
#18519=CARTESIAN_POINT('',(15.,0.,-8.5));
#18520=CARTESIAN_POINT('Origin',(11.,0.,-8.5));
#18521=CARTESIAN_POINT('',(15.,0.,8.5));
#18522=CARTESIAN_POINT('',(15.,0.,12.5));
#18523=CARTESIAN_POINT('',(11.,0.,12.5));
#18524=CARTESIAN_POINT('Origin',(11.,0.,8.5));
#18525=CARTESIAN_POINT('',(-11.,0.,12.5));
#18526=CARTESIAN_POINT('',(15.,0.,12.5));
#18527=CARTESIAN_POINT('Origin',(-11.,0.,8.50000000000001));
#18528=CARTESIAN_POINT('',(-4.2,0.,-3.2));
#18529=CARTESIAN_POINT('',(-4.2,0.,3.2));
#18530=CARTESIAN_POINT('',(-4.2,0.,3.2));
#18531=CARTESIAN_POINT('',(4.2,0.,3.2));
#18532=CARTESIAN_POINT('',(4.2,0.,3.2));
#18533=CARTESIAN_POINT('',(4.2,0.,-3.2));
#18534=CARTESIAN_POINT('',(4.2,0.,3.2));
#18535=CARTESIAN_POINT('',(4.2,0.,-3.2));
#18536=CARTESIAN_POINT('Origin',(-15.,6.,12.5));
#18537=CARTESIAN_POINT('',(-15.,6.,-8.49999999999999));
#18538=CARTESIAN_POINT('',(-15.,6.,8.50000000000001));
#18539=CARTESIAN_POINT('Origin',(15.,6.,12.5));
#18540=CARTESIAN_POINT('',(-11.,6.,12.5));
#18541=CARTESIAN_POINT('',(11.,6.,12.5));
#18542=CARTESIAN_POINT('Origin',(15.,6.,12.5));
#18543=CARTESIAN_POINT('',(15.,6.,-8.5));
#18544=CARTESIAN_POINT('',(15.,6.,8.5));
#18545=CARTESIAN_POINT('Origin',(15.,6.,-12.5));
#18546=CARTESIAN_POINT('',(-11.,6.,-12.5));
#18547=CARTESIAN_POINT('',(11.,6.,-12.5));
#18548=CARTESIAN_POINT('Origin',(-4.2,6.,3.2));
#18549=CARTESIAN_POINT('',(-4.2,6.,-3.2));
#18550=CARTESIAN_POINT('',(-4.2,6.,3.2));
#18551=CARTESIAN_POINT('Origin',(4.2,6.,3.2));
#18552=CARTESIAN_POINT('',(4.2,6.,3.2));
#18553=CARTESIAN_POINT('Origin',(4.2,6.,3.2));
#18554=CARTESIAN_POINT('',(4.2,6.,-3.2));
#18555=CARTESIAN_POINT('Origin',(4.2,6.,-3.2));
#18556=CARTESIAN_POINT('Origin',(-11.,6.,-8.49999999999999));
#18557=CARTESIAN_POINT('Origin',(11.,6.,-8.5));
#18558=CARTESIAN_POINT('Origin',(-11.,6.,8.50000000000001));
#18559=CARTESIAN_POINT('Origin',(11.,6.,8.5));
#18560=CARTESIAN_POINT('',(0.,0.,0.));
#18561=CARTESIAN_POINT('Origin',(0.,0.,37.));
#18562=CARTESIAN_POINT('',(-9.,-1.10218211923262E-15,-27.));
#18563=CARTESIAN_POINT('Origin',(0.,0.,-27.));
#18564=CARTESIAN_POINT('',(-9.,-1.10218211923262E-15,27.));
#18565=CARTESIAN_POINT('',(-9.,-1.10218211923262E-15,37.));
#18566=CARTESIAN_POINT('Origin',(0.,0.,27.));
#18567=CARTESIAN_POINT('Origin',(0.,0.,-1.45716771982052E-13));
#18568=CARTESIAN_POINT('',(12.7,1.55530143491714E-15,-1.45716771982052E-13));
#18569=CARTESIAN_POINT('',(-12.7,-1.55530143491714E-15,-1.45716771982052E-13));
#18570=CARTESIAN_POINT('Origin',(0.,0.,-1.45716771982052E-13));
#18571=CARTESIAN_POINT('Origin',(0.,0.,-1.45716771982052E-13));
#18572=CARTESIAN_POINT('',(-12.,-1.46957615897682E-15,-36.));
#18573=CARTESIAN_POINT('',(-12.7,-1.55530143491714E-15,-1.45716771982052E-13));
#18574=CARTESIAN_POINT('Origin',(0.,0.,-36.));
#18575=CARTESIAN_POINT('Origin',(0.,0.,-1.45716771982052E-13));
#18576=CARTESIAN_POINT('',(12.,-1.46957615897682E-15,36.));
#18577=CARTESIAN_POINT('',(12.7,-1.55530143491714E-15,-1.45716771982052E-13));
#18578=CARTESIAN_POINT('Origin',(0.,0.,36.));
#18579=CARTESIAN_POINT('Origin',(0.,0.,-37.));
#18580=CARTESIAN_POINT('',(-6.2,-7.59281015471359E-16,-36.));
#18581=CARTESIAN_POINT('Origin',(0.,0.,-36.));
#18582=CARTESIAN_POINT('',(-6.2,-7.59281015471359E-16,-37.));
#18583=CARTESIAN_POINT('',(-6.2,-7.59281015471359E-16,-37.));
#18584=CARTESIAN_POINT('Origin',(0.,0.,-37.));
#18585=CARTESIAN_POINT('Origin',(0.,0.,37.));
#18586=CARTESIAN_POINT('',(6.2,-7.59281015471359E-16,36.));
#18587=CARTESIAN_POINT('Origin',(0.,0.,36.));
#18588=CARTESIAN_POINT('',(6.2,-7.59281015471359E-16,37.));
#18589=CARTESIAN_POINT('',(6.2,-7.59281015471359E-16,37.));
#18590=CARTESIAN_POINT('Origin',(0.,0.,37.));
#18591=CARTESIAN_POINT('Origin',(0.,0.,36.));
#18592=CARTESIAN_POINT('',(4.2,-5.14351655641888E-16,-27.));
#18593=CARTESIAN_POINT('Origin',(0.,0.,-27.));
#18594=CARTESIAN_POINT('',(4.2,-5.14351655641888E-16,-37.));
#18595=CARTESIAN_POINT('',(4.2,-5.14351655641888E-16,36.));
#18596=CARTESIAN_POINT('Origin',(0.,0.,-37.));
#18597=CARTESIAN_POINT('Origin',(0.,0.,36.));
#18598=CARTESIAN_POINT('',(4.2,-5.14351655641888E-16,37.));
#18599=CARTESIAN_POINT('Origin',(0.,0.,37.));
#18600=CARTESIAN_POINT('',(4.2,-5.14351655641888E-16,27.));
#18601=CARTESIAN_POINT('',(4.2,-5.14351655641888E-16,36.));
#18602=CARTESIAN_POINT('Origin',(0.,0.,27.));
#18603=CARTESIAN_POINT('Origin',(0.,0.,-36.));
#18604=CARTESIAN_POINT('Origin',(0.,0.,36.));
#18605=CARTESIAN_POINT('Origin',(0.,0.,37.));
#18606=CARTESIAN_POINT('Origin',(0.,0.,-37.));
#18607=CARTESIAN_POINT('Origin',(0.,0.,27.));
#18608=CARTESIAN_POINT('Origin',(0.,0.,-27.));
#18609=CARTESIAN_POINT('',(0.,0.,0.));
#18610=CARTESIAN_POINT('Origin',(3.5,4.582650043662,-5.74646139614));
#18611=CARTESIAN_POINT('',(3.5,4.582650043662,-7.73096139614));
#18612=CARTESIAN_POINT('',(3.5,4.582650043662,-3.76196139614));
#18613=CARTESIAN_POINT('Origin',(3.5,4.582650043662,-5.74646139614));
#18614=CARTESIAN_POINT('Origin',(3.5,-1.635528864579,-7.165720154536));
#18615=CARTESIAN_POINT('',(3.5,-1.635528864579,-9.150220154536));
#18616=CARTESIAN_POINT('',(3.5,-1.635528864579,-5.181220154536));
#18617=CARTESIAN_POINT('Origin',(3.5,-1.635528864579,-7.165720154536));
#18618=CARTESIAN_POINT('Origin',(3.5,-6.622121179083,-3.189045482514));
#18619=CARTESIAN_POINT('',(3.5,-6.622121179083,-5.173545482514));
#18620=CARTESIAN_POINT('',(3.5,-6.622121179083,-1.204545482514));
#18621=CARTESIAN_POINT('Origin',(3.5,-6.622121179083,-3.189045482514));
#18622=CARTESIAN_POINT('Origin',(3.5,-6.622121179083,3.189045482514));
#18623=CARTESIAN_POINT('',(3.5,-6.622121179083,1.204545482514));
#18624=CARTESIAN_POINT('',(3.5,-6.622121179083,5.173545482514));
#18625=CARTESIAN_POINT('Origin',(3.5,-6.622121179083,3.189045482514));
#18626=CARTESIAN_POINT('Origin',(3.5,-1.635528864579,7.165720154536));
#18627=CARTESIAN_POINT('',(3.5,-1.635528864579,5.181220154536));
#18628=CARTESIAN_POINT('',(3.5,-1.635528864579,9.150220154536));
#18629=CARTESIAN_POINT('Origin',(3.5,-1.635528864579,7.165720154536));
#18630=CARTESIAN_POINT('Origin',(3.5,4.582650043662,5.74646139614));
#18631=CARTESIAN_POINT('',(3.5,4.582650043662,3.76196139614));
#18632=CARTESIAN_POINT('',(3.5,4.582650043662,7.73096139614));
#18633=CARTESIAN_POINT('Origin',(3.5,4.582650043662,5.74646139614));
#18634=CARTESIAN_POINT('Origin',(3.5,7.35,0.));
#18635=CARTESIAN_POINT('',(3.5,7.35,-1.9845));
#18636=CARTESIAN_POINT('',(3.5,7.35,1.9845));
#18637=CARTESIAN_POINT('Origin',(3.5,7.35,0.));
#18638=CARTESIAN_POINT('Origin',(0.3,0.,0.));
#18639=CARTESIAN_POINT('',(0.3,1.34711147906209E-15,-11.));
#18640=CARTESIAN_POINT('Origin',(0.3,0.,0.));
#18641=CARTESIAN_POINT('',(0.,1.31037207508767E-15,-10.7));
#18642=CARTESIAN_POINT('Origin',(0.3,1.31037207508767E-15,-10.7));
#18643=CARTESIAN_POINT('Origin',(0.,0.,0.));
#18644=CARTESIAN_POINT('Origin',(50.,0.,0.));
#18645=CARTESIAN_POINT('',(6.7,1.34711147906209E-15,-11.));
#18646=CARTESIAN_POINT('Origin',(6.7,0.,0.));
#18647=CARTESIAN_POINT('',(50.,1.34711147906209E-15,-11.));
#18648=CARTESIAN_POINT('Origin',(6.7,0.,0.));
#18649=CARTESIAN_POINT('',(7.,1.31037207508767E-15,-10.7));
#18650=CARTESIAN_POINT('Origin',(7.,0.,0.));
#18651=CARTESIAN_POINT('Origin',(6.7,1.31037207508767E-15,-10.7));
#18652=CARTESIAN_POINT('Origin',(50.,0.,0.));
#18653=CARTESIAN_POINT('',(6.91,1.17566092718146E-15,-9.6));
#18654=CARTESIAN_POINT('Origin',(6.91,0.,0.));
#18655=CARTESIAN_POINT('',(7.,1.17566092718146E-15,-9.6));
#18656=CARTESIAN_POINT('',(50.,1.17566092718146E-15,-9.6));
#18657=CARTESIAN_POINT('Origin',(7.,0.,0.));
#18658=CARTESIAN_POINT('Origin',(6.73,0.,0.));
#18659=CARTESIAN_POINT('',(6.55,1.17566092718146E-15,-9.6));
#18660=CARTESIAN_POINT('Origin',(6.55,0.,0.));
#18661=CARTESIAN_POINT('Origin',(6.73,1.17566092718146E-15,-9.6));
#18662=CARTESIAN_POINT('Origin',(6.40893841543323,0.,0.));
#18663=CARTESIAN_POINT('',(6.40893841543323,1.07768918324967E-15,-8.8));
#18664=CARTESIAN_POINT('Origin',(6.40893841543323,0.,0.));
#18665=CARTESIAN_POINT('',(6.40893841543323,1.07768918324967E-15,-8.8));
#18666=CARTESIAN_POINT('Origin',(50.,0.,0.));
#18667=CARTESIAN_POINT('',(4.85489492212496,1.07768918324967E-15,-8.8));
#18668=CARTESIAN_POINT('Origin',(4.85489492212496,0.,0.));
#18669=CARTESIAN_POINT('',(50.,1.07768918324967E-15,-8.8));
#18670=CARTESIAN_POINT('Origin',(3.5,0.,0.));
#18671=CARTESIAN_POINT('',(2.14510507787504,1.07768918324967E-15,-8.8));
#18672=CARTESIAN_POINT('Origin',(2.14510507787504,0.,0.));
#18673=CARTESIAN_POINT('Origin',(3.5,9.00115397373305E-16,-7.35));
#18674=CARTESIAN_POINT('Origin',(50.,0.,0.));
#18675=CARTESIAN_POINT('',(0.591061584566767,-1.12667505521557E-15,8.8));
#18676=CARTESIAN_POINT('',(0.59106158456677,1.07768918324967E-15,-8.8));
#18677=CARTESIAN_POINT('Origin',(0.591061584566767,0.,0.));
#18678=CARTESIAN_POINT('Origin',(0.591061584566767,0.,0.));
#18679=CARTESIAN_POINT('',(50.,1.07768918324967E-15,-8.8));
#18680=CARTESIAN_POINT('Origin',(0.45,0.,0.));
#18681=CARTESIAN_POINT('',(0.45,1.17566092718146E-15,9.6));
#18682=CARTESIAN_POINT('',(0.45,1.17566092718146E-15,9.6));
#18683=CARTESIAN_POINT('',(0.45,-1.17566092718146E-15,-9.6));
#18684=CARTESIAN_POINT('Origin',(0.45,0.,0.));
#18685=CARTESIAN_POINT('Origin',(0.45,0.,0.));
#18686=CARTESIAN_POINT('Origin',(0.27,0.,0.));
#18687=CARTESIAN_POINT('',(0.09,1.17566092718146E-15,-9.6));
#18688=CARTESIAN_POINT('Origin',(0.09,0.,0.));
#18689=CARTESIAN_POINT('Origin',(0.27,1.17566092718146E-15,-9.6));
#18690=CARTESIAN_POINT('Origin',(50.,0.,0.));
#18691=CARTESIAN_POINT('',(0.,1.17566092718146E-15,-9.6));
#18692=CARTESIAN_POINT('Origin',(0.,0.,0.));
#18693=CARTESIAN_POINT('',(50.,1.17566092718146E-15,-9.6));
#18694=CARTESIAN_POINT('Origin',(-3.25260651745651E-16,-10.7,0.));
#18695=CARTESIAN_POINT('Origin',(7.,-9.6,0.));
#18696=CARTESIAN_POINT('Origin',(3.5,0.,0.));
#18697=CARTESIAN_POINT('',(5.020728526069,-7.43972930482017E-16,-6.075));
#18698=CARTESIAN_POINT('Origin',(5.020728526069,0.,0.));
#18699=CARTESIAN_POINT('',(1.979271473931,7.43972930482017E-16,-6.075));
#18700=CARTESIAN_POINT('Origin',(3.5,9.00115397373305E-16,-7.35));
#18701=CARTESIAN_POINT('Origin',(1.979271473931,0.,0.));
#18702=CARTESIAN_POINT('Origin',(6.64,0.,0.));
#18703=CARTESIAN_POINT('',(6.64,1.17566092718146E-15,-9.6));
#18704=CARTESIAN_POINT('Origin',(6.64,0.,0.));
#18705=CARTESIAN_POINT('',(6.55,1.0677389280066E-15,-8.71875));
#18706=CARTESIAN_POINT('',(6.64,1.17566092718146E-15,-9.6));
#18707=CARTESIAN_POINT('Origin',(6.55,0.,0.));
#18708=CARTESIAN_POINT('Origin',(50.,0.,0.));
#18709=CARTESIAN_POINT('',(6.73,1.17566092718146E-15,-9.6));
#18710=CARTESIAN_POINT('Origin',(6.73,0.,0.));
#18711=CARTESIAN_POINT('',(50.,1.17566092718146E-15,-9.6));
#18712=CARTESIAN_POINT('Origin',(6.685,0.,0.));
#18713=CARTESIAN_POINT('',(6.685,-1.06773892800661E-15,8.71875000000007));
#18714=CARTESIAN_POINT('',(6.685,1.0677389280066E-15,-8.71875));
#18715=CARTESIAN_POINT('Origin',(6.685,0.,0.));
#18716=CARTESIAN_POINT('Origin',(6.685,0.,0.));
#18717=CARTESIAN_POINT('',(6.685,1.0677389280066E-15,-8.71875));
#18718=CARTESIAN_POINT('Origin',(6.73,0.,0.));
#18719=CARTESIAN_POINT('',(6.73,9.59816928831738E-16,7.8375));
#18720=CARTESIAN_POINT('',(6.73,9.59816928831738E-16,7.8375));
#18721=CARTESIAN_POINT('Origin',(6.73,0.,0.));
#18722=CARTESIAN_POINT('Origin',(6.55,0.,0.));
#18723=CARTESIAN_POINT('',(6.64,-7.43972930482017E-16,-6.075));
#18724=CARTESIAN_POINT('',(6.63999999999999,7.43972930482017E-16,6.075));
#18725=CARTESIAN_POINT('Origin',(6.64,0.,0.));
#18726=CARTESIAN_POINT('',(6.55,9.59816928831738E-16,7.8375));
#18727=CARTESIAN_POINT('',(6.55,9.59816928831738E-16,7.8375));
#18728=CARTESIAN_POINT('Origin',(6.55,0.,0.));
#18729=CARTESIAN_POINT('Origin',(6.64,0.,0.));
#18730=CARTESIAN_POINT('Origin',(0.45,0.,0.));
#18731=CARTESIAN_POINT('',(0.36,-1.17566092718146E-15,-9.6));
#18732=CARTESIAN_POINT('',(0.36,1.17566092718146E-15,9.6));
#18733=CARTESIAN_POINT('Origin',(0.36,0.,0.));
#18734=CARTESIAN_POINT('',(0.45,1.0677389280066E-15,8.71875));
#18735=CARTESIAN_POINT('',(0.45,1.0677389280066E-15,8.71875));
#18736=CARTESIAN_POINT('Origin',(0.45,0.,0.));
#18737=CARTESIAN_POINT('Origin',(0.36,0.,0.));
#18738=CARTESIAN_POINT('Origin',(0.36,0.,0.));
#18739=CARTESIAN_POINT('',(0.36,7.43972930482017E-16,-6.075));
#18740=CARTESIAN_POINT('Origin',(0.36,0.,0.));
#18741=CARTESIAN_POINT('',(0.449999999999993,9.59816928831738E-16,-7.8375));
#18742=CARTESIAN_POINT('',(0.36,7.43972930482017E-16,-6.075));
#18743=CARTESIAN_POINT('Origin',(0.45,0.,0.));
#18744=CARTESIAN_POINT('Origin',(0.315,0.,0.));
#18745=CARTESIAN_POINT('',(0.315,-1.12169992759403E-15,8.71875));
#18746=CARTESIAN_POINT('',(0.315,1.0677389280066E-15,-8.71875));
#18747=CARTESIAN_POINT('Origin',(0.315,0.,0.));
#18748=CARTESIAN_POINT('Origin',(0.315,0.,0.));
#18749=CARTESIAN_POINT('',(0.269999999999995,9.59816928831738E-16,-7.8375));
#18750=CARTESIAN_POINT('',(0.315,1.0677389280066E-15,-8.71875));
#18751=CARTESIAN_POINT('Origin',(0.27,0.,0.));
#18752=CARTESIAN_POINT('Origin',(0.27,0.,0.));
#18753=CARTESIAN_POINT('',(0.27,1.17566092718146E-15,9.6));
#18754=CARTESIAN_POINT('',(0.27,1.17566092718146E-15,9.6));
#18755=CARTESIAN_POINT('',(0.27,-1.17566092718146E-15,-9.6));
#18756=CARTESIAN_POINT('Origin',(0.27,0.,0.));
#18757=CARTESIAN_POINT('Origin',(0.27,0.,0.));
#18758=CARTESIAN_POINT('Origin',(50.,0.,0.));
#18759=CARTESIAN_POINT('',(50.,1.17566092718146E-15,-9.6));
#18760=CARTESIAN_POINT('Origin',(50.,0.,0.));
#18761=CARTESIAN_POINT('',(50.,7.43972930482017E-16,-6.075));
#18762=CARTESIAN_POINT('Origin',(50.,0.,0.));
#18763=CARTESIAN_POINT('',(6.9,7.43972930482017E-16,-6.075));
#18764=CARTESIAN_POINT('Origin',(6.9,0.,0.));
#18765=CARTESIAN_POINT('',(6.73,7.43972930482017E-16,-6.075));
#18766=CARTESIAN_POINT('',(50.,7.43972930482017E-16,-6.075));
#18767=CARTESIAN_POINT('Origin',(6.73,0.,0.));
#18768=CARTESIAN_POINT('Origin',(6.9,0.,0.));
#18769=CARTESIAN_POINT('',(7.,7.31726462490544E-16,-5.975));
#18770=CARTESIAN_POINT('Origin',(7.,0.,0.));
#18771=CARTESIAN_POINT('Origin',(6.9,7.31726462490544E-16,-5.975));
#18772=CARTESIAN_POINT('Origin',(6.7,0.,0.));
#18773=CARTESIAN_POINT('',(6.7,4.89858719658941E-16,-4.));
#18774=CARTESIAN_POINT('Origin',(6.7,0.,0.));
#18775=CARTESIAN_POINT('',(7.,5.26598123633362E-16,-4.3));
#18776=CARTESIAN_POINT('Origin',(6.7,5.26598123633362E-16,-4.3));
#18777=CARTESIAN_POINT('Origin',(7.,0.,0.));
#18778=CARTESIAN_POINT('Origin',(50.,0.,0.));
#18779=CARTESIAN_POINT('',(0.300000000000002,4.89858719658941E-16,-4.));
#18780=CARTESIAN_POINT('Origin',(0.3,0.,0.));
#18781=CARTESIAN_POINT('',(50.,4.89858719658941E-16,-4.));
#18782=CARTESIAN_POINT('Origin',(0.3,0.,0.));
#18783=CARTESIAN_POINT('',(0.,5.26598123633362E-16,-4.3));
#18784=CARTESIAN_POINT('Origin',(0.,0.,0.));
#18785=CARTESIAN_POINT('Origin',(0.3,5.26598123633362E-16,-4.3));
#18786=CARTESIAN_POINT('Origin',(0.1,0.,0.));
#18787=CARTESIAN_POINT('',(0.100000000000003,7.43972930482017E-16,-6.075));
#18788=CARTESIAN_POINT('Origin',(0.100000000000003,0.,0.));
#18789=CARTESIAN_POINT('',(0.,7.31726462490544E-16,-5.975));
#18790=CARTESIAN_POINT('Origin',(0.1,7.31726462490544E-16,-5.975));
#18791=CARTESIAN_POINT('Origin',(0.,0.,0.));
#18792=CARTESIAN_POINT('Origin',(50.,0.,0.));
#18793=CARTESIAN_POINT('',(0.27000000000001,7.43972930482017E-16,-6.075));
#18794=CARTESIAN_POINT('Origin',(0.27,0.,0.));
#18795=CARTESIAN_POINT('',(50.,7.43972930482017E-16,-6.075));
#18796=CARTESIAN_POINT('Origin',(50.,0.,0.));
#18797=CARTESIAN_POINT('',(50.,7.43972930482017E-16,-6.075));
#18798=CARTESIAN_POINT('Origin',(0.,-5.975,0.));
#18799=CARTESIAN_POINT('Origin',(7.,-4.3,0.));
#18800=CARTESIAN_POINT('Origin',(0.27,-7.8375,0.));
#18801=CARTESIAN_POINT('Origin',(0.45,-7.8375,0.));
#18802=CARTESIAN_POINT('Origin',(6.55,-8.71875,0.));
#18803=CARTESIAN_POINT('Origin',(6.73,-6.075,0.));
#18804=CARTESIAN_POINT('',(-190.,-20.0599999999996,71.5600000000024));
#18805=CARTESIAN_POINT('',(-5.55111512312578E-14,15.0000000000005,37.0000000000024));
#18806=CARTESIAN_POINT('',(-5.55111512312597E-14,15.,-37.0000000000023));
#18807=CARTESIAN_POINT('',(5.98861174095206E-14,14.9999999999998,37.0000000000024));
#18808=CARTESIAN_POINT('',(5.03483239160184E-14,15.,-36.9999999999976));
#18809=CARTESIAN_POINT('',(158.,15.0000000000006,2.40259201422788E-12));
#18810=CARTESIAN_POINT('',(140.381884337382,-2.00000000000002,-39.9999999999978));
#18811=CARTESIAN_POINT('',(-91.3911565890686,-37.9999999999997,43.0000000000022));
#18812=CARTESIAN_POINT('',(182.5,-16.4999999999994,45.5000000000024));
#18813=CARTESIAN_POINT('',(171.25,-16.5000000000044,54.500000000001));
#18814=CARTESIAN_POINT('',(212.,17.5,54.500000000001));
#18815=CARTESIAN_POINT('',(212.,17.5,2.39741103073633E-12));
#18816=CARTESIAN_POINT('',(160.,-5.18436211685224,27.5000000000024));
#18817=CARTESIAN_POINT('',(212.061712730758,17.3142588855908,54.500000000001));
#18818=CARTESIAN_POINT('',(212.,17.5,-36.9999999999976));
#18819=CARTESIAN_POINT('',(1.00000000000008,17.4999999999989,0.));
#18820=CARTESIAN_POINT('',(-190.,-20.0599999999999,121.560000000002));
#18821=CARTESIAN_POINT('',(-158.,15.0000000000006,2.39565312032397E-12));
#18822=CARTESIAN_POINT('',(-91.3911565890686,-1.99999999999973,40.0000000000022));
#18823=CARTESIAN_POINT('',(140.381884337382,-1.99999999999973,40.0000000000022));
#18824=CARTESIAN_POINT('',(-91.3911565890686,-2.00000000000003,-39.9999999999978));
#18825=CARTESIAN_POINT('',(140.381884337382,-37.9999999999997,43.0000000000022));
#18826=CARTESIAN_POINT('',(140.381884337382,-38.,-42.9999999999977));
#18827=CARTESIAN_POINT('',(-91.3911565890686,-38.,-42.9999999999978));
#18828=CARTESIAN_POINT('',(-210.,17.4999999999998,2.36354922848523E-12));
#18829=CARTESIAN_POINT('',(212.,17.5000000000005,37.0000000000024));
#18830=CARTESIAN_POINT('',(-210.,17.4999999999999,37.0000000000024));
#18831=CARTESIAN_POINT('',(-210.,17.5,-36.9999999999976));
#18832=UNCERTAINTY_MEASURE_WITH_UNIT(LENGTH_MEASURE(0.01),#18868,
'DISTANCE_ACCURACY_VALUE',
'Maximum model space distance between geometric entities at asserted c
onnectivities');
#18833=UNCERTAINTY_MEASURE_WITH_UNIT(LENGTH_MEASURE(0.01),#18868,
'DISTANCE_ACCURACY_VALUE',
'Maximum model space distance between geometric entities at asserted c
onnectivities');
#18834=UNCERTAINTY_MEASURE_WITH_UNIT(LENGTH_MEASURE(0.01),#18868,
'DISTANCE_ACCURACY_VALUE',
'Maximum model space distance between geometric entities at asserted c
onnectivities');
#18835=UNCERTAINTY_MEASURE_WITH_UNIT(LENGTH_MEASURE(0.01),#18868,
'DISTANCE_ACCURACY_VALUE',
'Maximum model space distance between geometric entities at asserted c
onnectivities');
#18836=UNCERTAINTY_MEASURE_WITH_UNIT(LENGTH_MEASURE(0.01),#18868,
'DISTANCE_ACCURACY_VALUE',
'Maximum model space distance between geometric entities at asserted c
onnectivities');
#18837=UNCERTAINTY_MEASURE_WITH_UNIT(LENGTH_MEASURE(0.01),#18868,
'DISTANCE_ACCURACY_VALUE',
'Maximum model space distance between geometric entities at asserted c
onnectivities');
#18838=UNCERTAINTY_MEASURE_WITH_UNIT(LENGTH_MEASURE(0.01),#18868,
'DISTANCE_ACCURACY_VALUE',
'Maximum model space distance between geometric entities at asserted c
onnectivities');
#18839=UNCERTAINTY_MEASURE_WITH_UNIT(LENGTH_MEASURE(0.01),#18868,
'DISTANCE_ACCURACY_VALUE',
'Maximum model space distance between geometric entities at asserted c
onnectivities');
#18840=UNCERTAINTY_MEASURE_WITH_UNIT(LENGTH_MEASURE(0.01),#18868,
'DISTANCE_ACCURACY_VALUE',
'Maximum model space distance between geometric entities at asserted c
onnectivities');
#18841=UNCERTAINTY_MEASURE_WITH_UNIT(LENGTH_MEASURE(0.01),#18868,
'DISTANCE_ACCURACY_VALUE',
'Maximum model space distance between geometric entities at asserted c
onnectivities');
#18842=UNCERTAINTY_MEASURE_WITH_UNIT(LENGTH_MEASURE(0.01),#18868,
'DISTANCE_ACCURACY_VALUE',
'Maximum model space distance between geometric entities at asserted c
onnectivities');
#18843=UNCERTAINTY_MEASURE_WITH_UNIT(LENGTH_MEASURE(0.01),#18868,
'DISTANCE_ACCURACY_VALUE',
'Maximum model space distance between geometric entities at asserted c
onnectivities');
#18844=UNCERTAINTY_MEASURE_WITH_UNIT(LENGTH_MEASURE(0.01),#18868,
'DISTANCE_ACCURACY_VALUE',
'Maximum model space distance between geometric entities at asserted c
onnectivities');
#18845=UNCERTAINTY_MEASURE_WITH_UNIT(LENGTH_MEASURE(0.01),#18868,
'DISTANCE_ACCURACY_VALUE',
'Maximum model space distance between geometric entities at asserted c
onnectivities');
#18846=UNCERTAINTY_MEASURE_WITH_UNIT(LENGTH_MEASURE(0.01),#18868,
'DISTANCE_ACCURACY_VALUE',
'Maximum model space distance between geometric entities at asserted c
onnectivities');
#18847=UNCERTAINTY_MEASURE_WITH_UNIT(LENGTH_MEASURE(0.01),#18868,
'DISTANCE_ACCURACY_VALUE',
'Maximum model space distance between geometric entities at asserted c
onnectivities');
#18848=UNCERTAINTY_MEASURE_WITH_UNIT(LENGTH_MEASURE(0.01),#18868,
'DISTANCE_ACCURACY_VALUE',
'Maximum model space distance between geometric entities at asserted c
onnectivities');
#18849=UNCERTAINTY_MEASURE_WITH_UNIT(LENGTH_MEASURE(0.01),#18868,
'DISTANCE_ACCURACY_VALUE',
'Maximum model space distance between geometric entities at asserted c
onnectivities');
#18850=(
GEOMETRIC_REPRESENTATION_CONTEXT(3)
GLOBAL_UNCERTAINTY_ASSIGNED_CONTEXT((#18832))
GLOBAL_UNIT_ASSIGNED_CONTEXT((#18868,#18870,#18871))
REPRESENTATION_CONTEXT('','3D')
);
#18851=(
GEOMETRIC_REPRESENTATION_CONTEXT(3)
GLOBAL_UNCERTAINTY_ASSIGNED_CONTEXT((#18833))
GLOBAL_UNIT_ASSIGNED_CONTEXT((#18868,#18870,#18871))
REPRESENTATION_CONTEXT('','3D')
);
#18852=(
GEOMETRIC_REPRESENTATION_CONTEXT(3)
GLOBAL_UNCERTAINTY_ASSIGNED_CONTEXT((#18834))
GLOBAL_UNIT_ASSIGNED_CONTEXT((#18868,#18870,#18871))
REPRESENTATION_CONTEXT('','3D')
);
#18853=(
GEOMETRIC_REPRESENTATION_CONTEXT(3)
GLOBAL_UNCERTAINTY_ASSIGNED_CONTEXT((#18835))
GLOBAL_UNIT_ASSIGNED_CONTEXT((#18868,#18870,#18871))
REPRESENTATION_CONTEXT('','3D')
);
#18854=(
GEOMETRIC_REPRESENTATION_CONTEXT(3)
GLOBAL_UNCERTAINTY_ASSIGNED_CONTEXT((#18836))
GLOBAL_UNIT_ASSIGNED_CONTEXT((#18868,#18870,#18871))
REPRESENTATION_CONTEXT('','3D')
);
#18855=(
GEOMETRIC_REPRESENTATION_CONTEXT(3)
GLOBAL_UNCERTAINTY_ASSIGNED_CONTEXT((#18837))
GLOBAL_UNIT_ASSIGNED_CONTEXT((#18868,#18870,#18871))
REPRESENTATION_CONTEXT('','3D')
);
#18856=(
GEOMETRIC_REPRESENTATION_CONTEXT(3)
GLOBAL_UNCERTAINTY_ASSIGNED_CONTEXT((#18838))
GLOBAL_UNIT_ASSIGNED_CONTEXT((#18868,#18870,#18871))
REPRESENTATION_CONTEXT('','3D')
);
#18857=(
GEOMETRIC_REPRESENTATION_CONTEXT(3)
GLOBAL_UNCERTAINTY_ASSIGNED_CONTEXT((#18839))
GLOBAL_UNIT_ASSIGNED_CONTEXT((#18868,#18870,#18871))
REPRESENTATION_CONTEXT('','3D')
);
#18858=(
GEOMETRIC_REPRESENTATION_CONTEXT(3)
GLOBAL_UNCERTAINTY_ASSIGNED_CONTEXT((#18840))
GLOBAL_UNIT_ASSIGNED_CONTEXT((#18868,#18870,#18871))
REPRESENTATION_CONTEXT('','3D')
);
#18859=(
GEOMETRIC_REPRESENTATION_CONTEXT(3)
GLOBAL_UNCERTAINTY_ASSIGNED_CONTEXT((#18841))
GLOBAL_UNIT_ASSIGNED_CONTEXT((#18868,#18870,#18871))
REPRESENTATION_CONTEXT('','3D')
);
#18860=(
GEOMETRIC_REPRESENTATION_CONTEXT(3)
GLOBAL_UNCERTAINTY_ASSIGNED_CONTEXT((#18842))
GLOBAL_UNIT_ASSIGNED_CONTEXT((#18868,#18870,#18871))
REPRESENTATION_CONTEXT('','3D')
);
#18861=(
GEOMETRIC_REPRESENTATION_CONTEXT(3)
GLOBAL_UNCERTAINTY_ASSIGNED_CONTEXT((#18843))
GLOBAL_UNIT_ASSIGNED_CONTEXT((#18868,#18870,#18871))
REPRESENTATION_CONTEXT('','3D')
);
#18862=(
GEOMETRIC_REPRESENTATION_CONTEXT(3)
GLOBAL_UNCERTAINTY_ASSIGNED_CONTEXT((#18844))
GLOBAL_UNIT_ASSIGNED_CONTEXT((#18868,#18870,#18871))
REPRESENTATION_CONTEXT('','3D')
);
#18863=(
GEOMETRIC_REPRESENTATION_CONTEXT(3)
GLOBAL_UNCERTAINTY_ASSIGNED_CONTEXT((#18845))
GLOBAL_UNIT_ASSIGNED_CONTEXT((#18868,#18870,#18871))
REPRESENTATION_CONTEXT('','3D')
);
#18864=(
GEOMETRIC_REPRESENTATION_CONTEXT(3)
GLOBAL_UNCERTAINTY_ASSIGNED_CONTEXT((#18846))
GLOBAL_UNIT_ASSIGNED_CONTEXT((#18868,#18870,#18871))
REPRESENTATION_CONTEXT('','3D')
);
#18865=(
GEOMETRIC_REPRESENTATION_CONTEXT(3)
GLOBAL_UNCERTAINTY_ASSIGNED_CONTEXT((#18847))
GLOBAL_UNIT_ASSIGNED_CONTEXT((#18868,#18870,#18871))
REPRESENTATION_CONTEXT('','3D')
);
#18866=(
GEOMETRIC_REPRESENTATION_CONTEXT(3)
GLOBAL_UNCERTAINTY_ASSIGNED_CONTEXT((#18848))
GLOBAL_UNIT_ASSIGNED_CONTEXT((#18868,#18870,#18871))
REPRESENTATION_CONTEXT('','3D')
);
#18867=(
GEOMETRIC_REPRESENTATION_CONTEXT(3)
GLOBAL_UNCERTAINTY_ASSIGNED_CONTEXT((#18849))
GLOBAL_UNIT_ASSIGNED_CONTEXT((#18868,#18870,#18871))
REPRESENTATION_CONTEXT('','3D')
);
#18868=(
LENGTH_UNIT()
NAMED_UNIT(*)
SI_UNIT(.MILLI.,.METRE.)
);
#18869=(
LENGTH_UNIT()
NAMED_UNIT(*)
SI_UNIT($,.METRE.)
);
#18870=(
NAMED_UNIT(*)
PLANE_ANGLE_UNIT()
SI_UNIT($,.RADIAN.)
);
#18871=(
NAMED_UNIT(*)
SI_UNIT($,.STERADIAN.)
SOLID_ANGLE_UNIT()
);
#18872=SHAPE_DEFINITION_REPRESENTATION(#18889,#18934);
#18873=SHAPE_DEFINITION_REPRESENTATION(#18890,#18935);
#18874=SHAPE_DEFINITION_REPRESENTATION(#18891,#18936);
#18875=SHAPE_DEFINITION_REPRESENTATION(#18892,#18937);
#18876=SHAPE_DEFINITION_REPRESENTATION(#18893,#18938);
#18877=SHAPE_DEFINITION_REPRESENTATION(#18894,#18939);
#18878=SHAPE_DEFINITION_REPRESENTATION(#18895,#18940);
#18879=SHAPE_DEFINITION_REPRESENTATION(#18896,#18941);
#18880=SHAPE_DEFINITION_REPRESENTATION(#18897,#18942);
#18881=SHAPE_DEFINITION_REPRESENTATION(#18898,#18943);
#18882=SHAPE_DEFINITION_REPRESENTATION(#18899,#18944);
#18883=SHAPE_DEFINITION_REPRESENTATION(#18900,#18945);
#18884=SHAPE_DEFINITION_REPRESENTATION(#18901,#18946);
#18885=SHAPE_DEFINITION_REPRESENTATION(#18902,#18947);
#18886=SHAPE_DEFINITION_REPRESENTATION(#18903,#18948);
#18887=SHAPE_DEFINITION_REPRESENTATION(#18904,#18949);
#18888=SHAPE_DEFINITION_REPRESENTATION(#18905,#18950);
#18889=PRODUCT_DEFINITION_SHAPE('',$,#18952);
#18890=PRODUCT_DEFINITION_SHAPE('',$,#18953);
#18891=PRODUCT_DEFINITION_SHAPE('',$,#18954);
#18892=PRODUCT_DEFINITION_SHAPE('',$,#18955);
#18893=PRODUCT_DEFINITION_SHAPE('',$,#18956);
#18894=PRODUCT_DEFINITION_SHAPE('',$,#18957);
#18895=PRODUCT_DEFINITION_SHAPE('',$,#18958);
#18896=PRODUCT_DEFINITION_SHAPE('',$,#18959);
#18897=PRODUCT_DEFINITION_SHAPE('',$,#18960);
#18898=PRODUCT_DEFINITION_SHAPE('',$,#18961);
#18899=PRODUCT_DEFINITION_SHAPE('',$,#18962);
#18900=PRODUCT_DEFINITION_SHAPE('',$,#18963);
#18901=PRODUCT_DEFINITION_SHAPE('',$,#18964);
#18902=PRODUCT_DEFINITION_SHAPE('',$,#18965);
#18903=PRODUCT_DEFINITION_SHAPE('',$,#18966);
#18904=PRODUCT_DEFINITION_SHAPE('',$,#18967);
#18905=PRODUCT_DEFINITION_SHAPE('',$,#18968);
#18906=PRODUCT_DEFINITION_SHAPE($,$,#95);
#18907=PRODUCT_DEFINITION_SHAPE($,$,#96);
#18908=PRODUCT_DEFINITION_SHAPE($,$,#97);
#18909=PRODUCT_DEFINITION_SHAPE($,$,#98);
#18910=PRODUCT_DEFINITION_SHAPE($,$,#99);
#18911=PRODUCT_DEFINITION_SHAPE($,$,#100);
#18912=PRODUCT_DEFINITION_SHAPE($,$,#101);
#18913=PRODUCT_DEFINITION_SHAPE($,$,#102);
#18914=PRODUCT_DEFINITION_SHAPE($,$,#103);
#18915=PRODUCT_DEFINITION_SHAPE($,$,#104);
#18916=PRODUCT_DEFINITION_SHAPE($,$,#105);
#18917=PRODUCT_DEFINITION_SHAPE($,$,#106);
#18918=PRODUCT_DEFINITION_SHAPE($,$,#107);
#18919=PRODUCT_DEFINITION_SHAPE($,$,#108);
#18920=PRODUCT_DEFINITION_SHAPE($,$,#109);
#18921=PRODUCT_DEFINITION_SHAPE($,$,#110);
#18922=PRODUCT_DEFINITION_SHAPE($,$,#111);
#18923=PRODUCT_DEFINITION_SHAPE($,$,#112);
#18924=PRODUCT_DEFINITION_SHAPE($,$,#113);
#18925=PRODUCT_DEFINITION_SHAPE($,$,#114);
#18926=PRODUCT_DEFINITION_SHAPE($,$,#115);
#18927=PRODUCT_DEFINITION_SHAPE($,$,#116);
#18928=PRODUCT_DEFINITION_SHAPE($,$,#117);
#18929=PRODUCT_DEFINITION_SHAPE($,$,#118);
#18930=PRODUCT_DEFINITION_SHAPE($,$,#119);
#18931=PRODUCT_DEFINITION_SHAPE($,$,#120);
#18932=PRODUCT_DEFINITION_SHAPE($,$,#121);
#18933=PRODUCT_DEFINITION_SHAPE($,$,#122);
#18934=SHAPE_REPRESENTATION('',(#11159,#12275,#12276,#12277,#12278,#12279,
#12280,#12281,#12282,#12283,#12284,#12285,#12286,#12287,#12288,#12289,#12290,
#12291,#12292,#12293,#12294,#12295,#12296,#12297,#12298,#12299,#12300,#12301,
#12302),#18850);
#18935=SHAPE_REPRESENTATION('',(#11160),#18851);
#18936=SHAPE_REPRESENTATION('',(#11233),#18852);
#18937=SHAPE_REPRESENTATION('',(#11306),#18853);
#18938=SHAPE_REPRESENTATION('',(#11366),#18854);
#18939=SHAPE_REPRESENTATION('',(#11426),#18855);
#18940=SHAPE_REPRESENTATION('',(#11511),#18856);
#18941=SHAPE_REPRESENTATION('',(#11547),#18857);
#18942=SHAPE_REPRESENTATION('',(#11578),#18858);
#18943=SHAPE_REPRESENTATION('',(#11670),#18859);
#18944=SHAPE_REPRESENTATION('',(#11689),#18860);
#18945=SHAPE_REPRESENTATION('',(#11712),#18861);
#18946=SHAPE_REPRESENTATION('',(#12015),#18862);
#18947=SHAPE_REPRESENTATION('',(#12084),#18863);
#18948=SHAPE_REPRESENTATION('',(#12112),#18864);
#18949=SHAPE_REPRESENTATION('',(#12135),#18865);
#18950=SHAPE_REPRESENTATION('',(#12163),#18866);
#18951=PRODUCT_DEFINITION_CONTEXT('part definition',#19004,'design');
#18952=PRODUCT_DEFINITION('MAT-034','MAT-034',#18969,#18951);
#18953=PRODUCT_DEFINITION('Drive End Bracket 1','Drive End Bracket 1',#18970,
#18951);
#18954=PRODUCT_DEFINITION('Drive End Bracket 2','Drive End Bracket 2',#18971,
#18951);
#18955=PRODUCT_DEFINITION('Idler End Bracket 1','Idler End Bracket 1',#18972,
#18951);
#18956=PRODUCT_DEFINITION('Idler End Bracket 2','Idler End Bracket 2',#18973,
#18951);
#18957=PRODUCT_DEFINITION('Motor Mounting Plate','Motor Mounting Plate',
#18974,#18951);
#18958=PRODUCT_DEFINITION('Motor Pulley','Motor Pulley',#18975,#18951);
#18959=PRODUCT_DEFINITION('driven pulley','Driven Pulley',#18976,#18951);
#18960=PRODUCT_DEFINITION('motor','Motor',#18977,#18951);
#18961=PRODUCT_DEFINITION('Motor Drive Belt','Motor Drive Belt',#18978,
#18951);
#18962=PRODUCT_DEFINITION('Conveyor Belt','Conveyor Belt',#18979,#18951);
#18963=PRODUCT_DEFINITION('Frame Side Rail','Frame Side Rail',#18980,#18951);
#18964=PRODUCT_DEFINITION('Arm Clamp Block','Arm Clamp Block',#18981,#18951);
#18965=PRODUCT_DEFINITION('Mounting Arm','Mounting Arm',#18982,#18951);
#18966=PRODUCT_DEFINITION('Mounting Foot Plate','Mounting Foot Plate',#18983,
#18951);
#18967=PRODUCT_DEFINITION('Roller Shaft','Roller Shaft',#18984,#18951);
#18968=PRODUCT_DEFINITION('Ball Bearing','Ball Bearing',#18985,#18951);
#18969=PRODUCT_DEFINITION_FORMATION('',$,#19006);
#18970=PRODUCT_DEFINITION_FORMATION('',$,#19007);
#18971=PRODUCT_DEFINITION_FORMATION('',$,#19008);
#18972=PRODUCT_DEFINITION_FORMATION('',$,#19009);
#18973=PRODUCT_DEFINITION_FORMATION('',$,#19010);
#18974=PRODUCT_DEFINITION_FORMATION('',$,#19011);
#18975=PRODUCT_DEFINITION_FORMATION('',$,#19012);
#18976=PRODUCT_DEFINITION_FORMATION('',$,#19013);
#18977=PRODUCT_DEFINITION_FORMATION('',$,#19014);
#18978=PRODUCT_DEFINITION_FORMATION('',$,#19015);
#18979=PRODUCT_DEFINITION_FORMATION('',$,#19016);
#18980=PRODUCT_DEFINITION_FORMATION('',$,#19017);
#18981=PRODUCT_DEFINITION_FORMATION('',$,#19018);
#18982=PRODUCT_DEFINITION_FORMATION('',$,#19019);
#18983=PRODUCT_DEFINITION_FORMATION('',$,#19020);
#18984=PRODUCT_DEFINITION_FORMATION('',$,#19021);
#18985=PRODUCT_DEFINITION_FORMATION('',$,#19022);
#18986=PRODUCT_RELATED_PRODUCT_CATEGORY('MAT-034','MAT-034',(#19006));
#18987=PRODUCT_RELATED_PRODUCT_CATEGORY('Drive End Bracket 1',
'Drive End Bracket 1',(#19007));
#18988=PRODUCT_RELATED_PRODUCT_CATEGORY('Drive End Bracket 2',
'Drive End Bracket 2',(#19008));
#18989=PRODUCT_RELATED_PRODUCT_CATEGORY('Idler End Bracket 1',
'Idler End Bracket 1',(#19009));
#18990=PRODUCT_RELATED_PRODUCT_CATEGORY('Idler End Bracket 2',
'Idler End Bracket 2',(#19010));
#18991=PRODUCT_RELATED_PRODUCT_CATEGORY('Motor Mounting Plate',
'Motor Mounting Plate',(#19011));
#18992=PRODUCT_RELATED_PRODUCT_CATEGORY('Motor Pulley','Motor Pulley',(#19012));
#18993=PRODUCT_RELATED_PRODUCT_CATEGORY('Driven Pulley','Driven Pulley',
(#19013));
#18994=PRODUCT_RELATED_PRODUCT_CATEGORY('Motor','Motor',(#19014));
#18995=PRODUCT_RELATED_PRODUCT_CATEGORY('Motor Drive Belt',
'Motor Drive Belt',(#19015));
#18996=PRODUCT_RELATED_PRODUCT_CATEGORY('Conveyor Belt','Conveyor Belt',
(#19016));
#18997=PRODUCT_RELATED_PRODUCT_CATEGORY('Frame Side Rail',
'Frame Side Rail',(#19017));
#18998=PRODUCT_RELATED_PRODUCT_CATEGORY('Arm Clamp Block',
'Arm Clamp Block',(#19018));
#18999=PRODUCT_RELATED_PRODUCT_CATEGORY('Mounting Arm','Mounting Arm',(#19019));
#19000=PRODUCT_RELATED_PRODUCT_CATEGORY('Mounting Foot Plate',
'Mounting Foot Plate',(#19020));
#19001=PRODUCT_RELATED_PRODUCT_CATEGORY('Roller Shaft','Roller Shaft',(#19021));
#19002=PRODUCT_RELATED_PRODUCT_CATEGORY('Ball Bearing','Ball Bearing',(#19022));
#19003=APPLICATION_PROTOCOL_DEFINITION('international standard',
'automotive_design',2009,#19004);
#19004=APPLICATION_CONTEXT(
'Core Data for Automotive Mechanical Design Process');
#19005=PRODUCT_CONTEXT('part definition',#19004,'mechanical');
#19006=PRODUCT('MAT-034','MAT-034','STEP AP214',(#19005));
#19007=PRODUCT('Drive End Bracket 1','Drive End Bracket 1',$,(#19005));
#19008=PRODUCT('Drive End Bracket 2','Drive End Bracket 2',$,(#19005));
#19009=PRODUCT('Idler End Bracket 1','Idler End Bracket 1',$,(#19005));
#19010=PRODUCT('Idler End Bracket 2','Idler End Bracket 2',$,(#19005));
#19011=PRODUCT('Motor Mounting Plate','Motor Mounting Plate',$,(#19005));
#19012=PRODUCT('Motor Pulley','Motor Pulley',$,(#19005));
#19013=PRODUCT('driven pulley','Driven Pulley',$,(#19005));
#19014=PRODUCT('motor','Motor',$,(#19005));
#19015=PRODUCT('Motor Drive Belt','Motor Drive Belt',$,(#19005));
#19016=PRODUCT('Conveyor Belt','Conveyor Belt',$,(#19005));
#19017=PRODUCT('Frame Side Rail','Frame Side Rail',$,(#19005));
#19018=PRODUCT('Arm Clamp Block','Arm Clamp Block',$,(#19005));
#19019=PRODUCT('Mounting Arm','Mounting Arm',$,(#19005));
#19020=PRODUCT('Mounting Foot Plate','Mounting Foot Plate',$,(#19005));
#19021=PRODUCT('Roller Shaft','Roller Shaft',$,(#19005));
#19022=PRODUCT('Ball Bearing','Ball Bearing',$,(#19005));
#19023=PRESENTATION_STYLE_ASSIGNMENT((#19029));
#19024=PRESENTATION_STYLE_ASSIGNMENT((#19030));
#19025=PRESENTATION_STYLE_ASSIGNMENT((#19031));
#19026=PRESENTATION_STYLE_ASSIGNMENT((#19032));
#19027=PRESENTATION_STYLE_ASSIGNMENT((#19033));
#19028=PRESENTATION_STYLE_ASSIGNMENT((#19034));
#19029=SURFACE_STYLE_USAGE(.BOTH.,#19035);
#19030=SURFACE_STYLE_USAGE(.BOTH.,#19036);
#19031=SURFACE_STYLE_USAGE(.BOTH.,#19037);
#19032=SURFACE_STYLE_USAGE(.BOTH.,#19038);
#19033=SURFACE_STYLE_USAGE(.BOTH.,#19039);
#19034=SURFACE_STYLE_USAGE(.BOTH.,#19040);
#19035=SURFACE_SIDE_STYLE('',(#19041));
#19036=SURFACE_SIDE_STYLE('',(#19042));
#19037=SURFACE_SIDE_STYLE('',(#19043));
#19038=SURFACE_SIDE_STYLE('',(#19044));
#19039=SURFACE_SIDE_STYLE('',(#19045));
#19040=SURFACE_SIDE_STYLE('',(#19046));
#19041=SURFACE_STYLE_FILL_AREA(#19047);
#19042=SURFACE_STYLE_FILL_AREA(#19048);
#19043=SURFACE_STYLE_FILL_AREA(#19049);
#19044=SURFACE_STYLE_FILL_AREA(#19050);
#19045=SURFACE_STYLE_FILL_AREA(#19051);
#19046=SURFACE_STYLE_FILL_AREA(#19052);
#19047=FILL_AREA_STYLE('Steel - Satin',(#19053));
#19048=FILL_AREA_STYLE('Opaque(20,51,87)',(#19054));
#19049=FILL_AREA_STYLE('Opaque(97,158,199)',(#19055));
#19050=FILL_AREA_STYLE('Opaque(227,224,212)',(#19056));
#19051=FILL_AREA_STYLE('Opaque(122,133,145)',(#19057));
#19052=FILL_AREA_STYLE('Opaque(31,36,43)',(#19058));
#19053=FILL_AREA_STYLE_COLOUR('Steel - Satin',#19059);
#19054=FILL_AREA_STYLE_COLOUR('Opaque(20,51,87)',#19060);
#19055=FILL_AREA_STYLE_COLOUR('Opaque(97,158,199)',#19061);
#19056=FILL_AREA_STYLE_COLOUR('Opaque(227,224,212)',#19062);
#19057=FILL_AREA_STYLE_COLOUR('Opaque(122,133,145)',#19063);
#19058=FILL_AREA_STYLE_COLOUR('Opaque(31,36,43)',#19064);
#19059=COLOUR_RGB('Steel - Satin',0.627450980392157,0.627450980392157,0.627450980392157);
#19060=COLOUR_RGB('Opaque(20,51,87)',0.0784313725490196,0.2,0.341176470588235);
#19061=COLOUR_RGB('Opaque(97,158,199)',0.380392156862745,0.619607843137255,
0.780392156862745);
#19062=COLOUR_RGB('Opaque(227,224,212)',0.890196078431372,0.87843137254902,
0.831372549019608);
#19063=COLOUR_RGB('Opaque(122,133,145)',0.47843137254902,0.52156862745098,
0.568627450980392);
#19064=COLOUR_RGB('Opaque(31,36,43)',0.12156862745098,0.141176470588235,
0.168627450980392);
ENDSEC;
END-ISO-10303-21;
